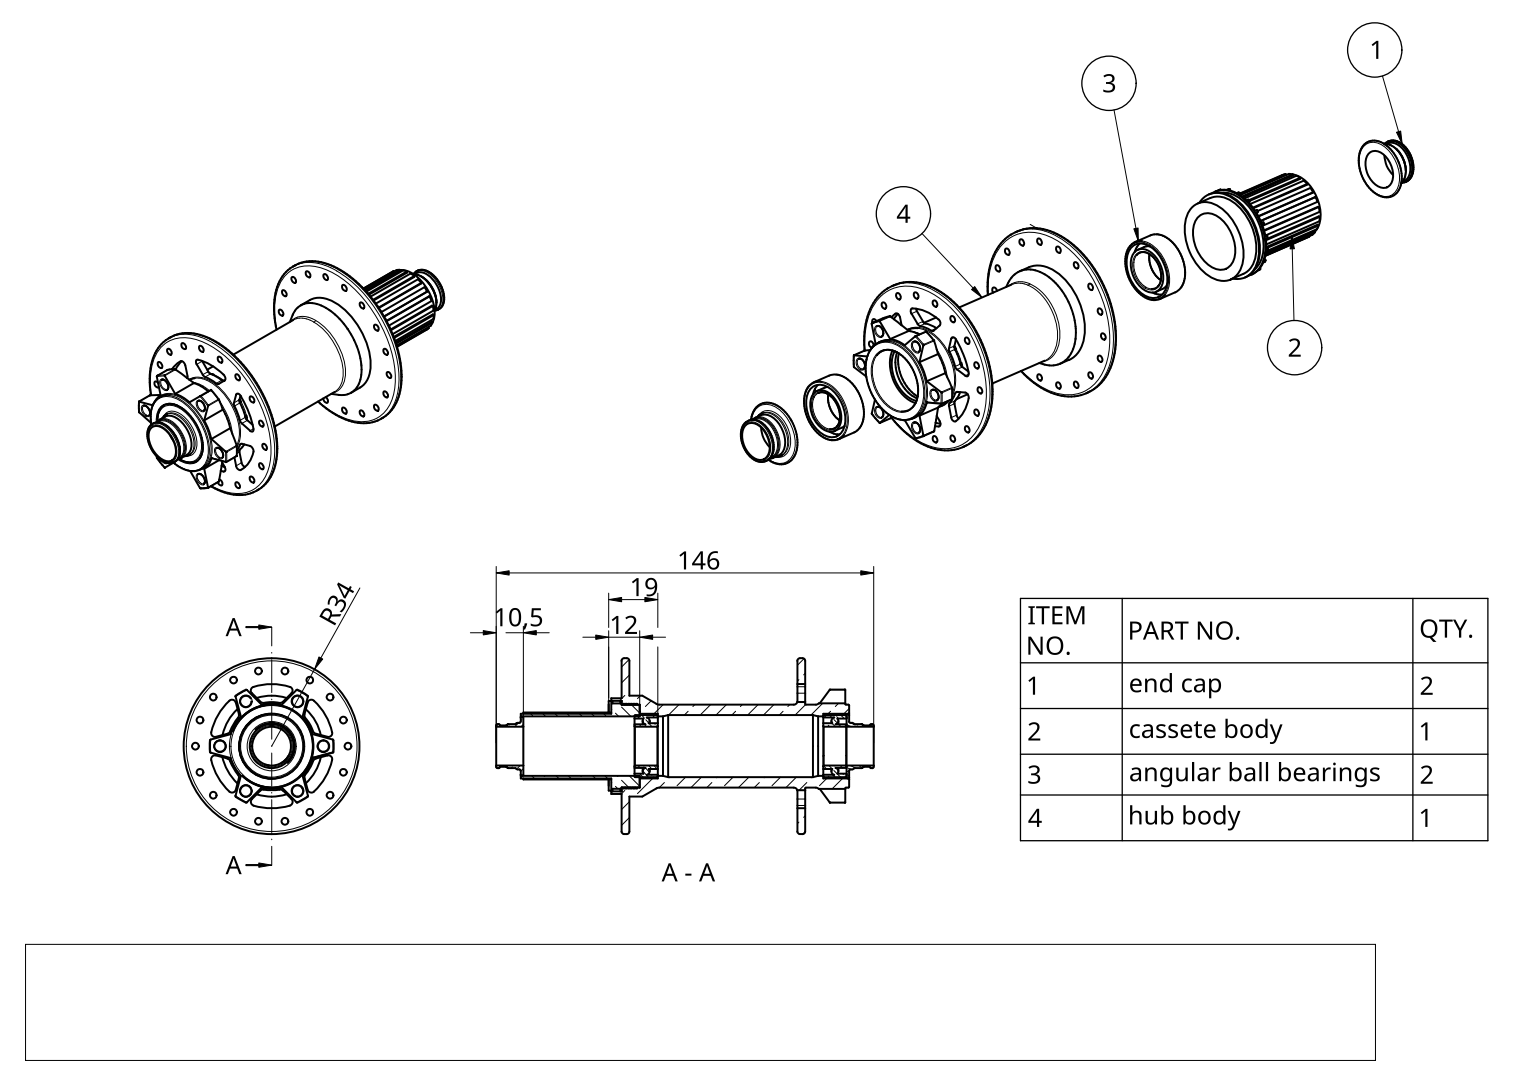
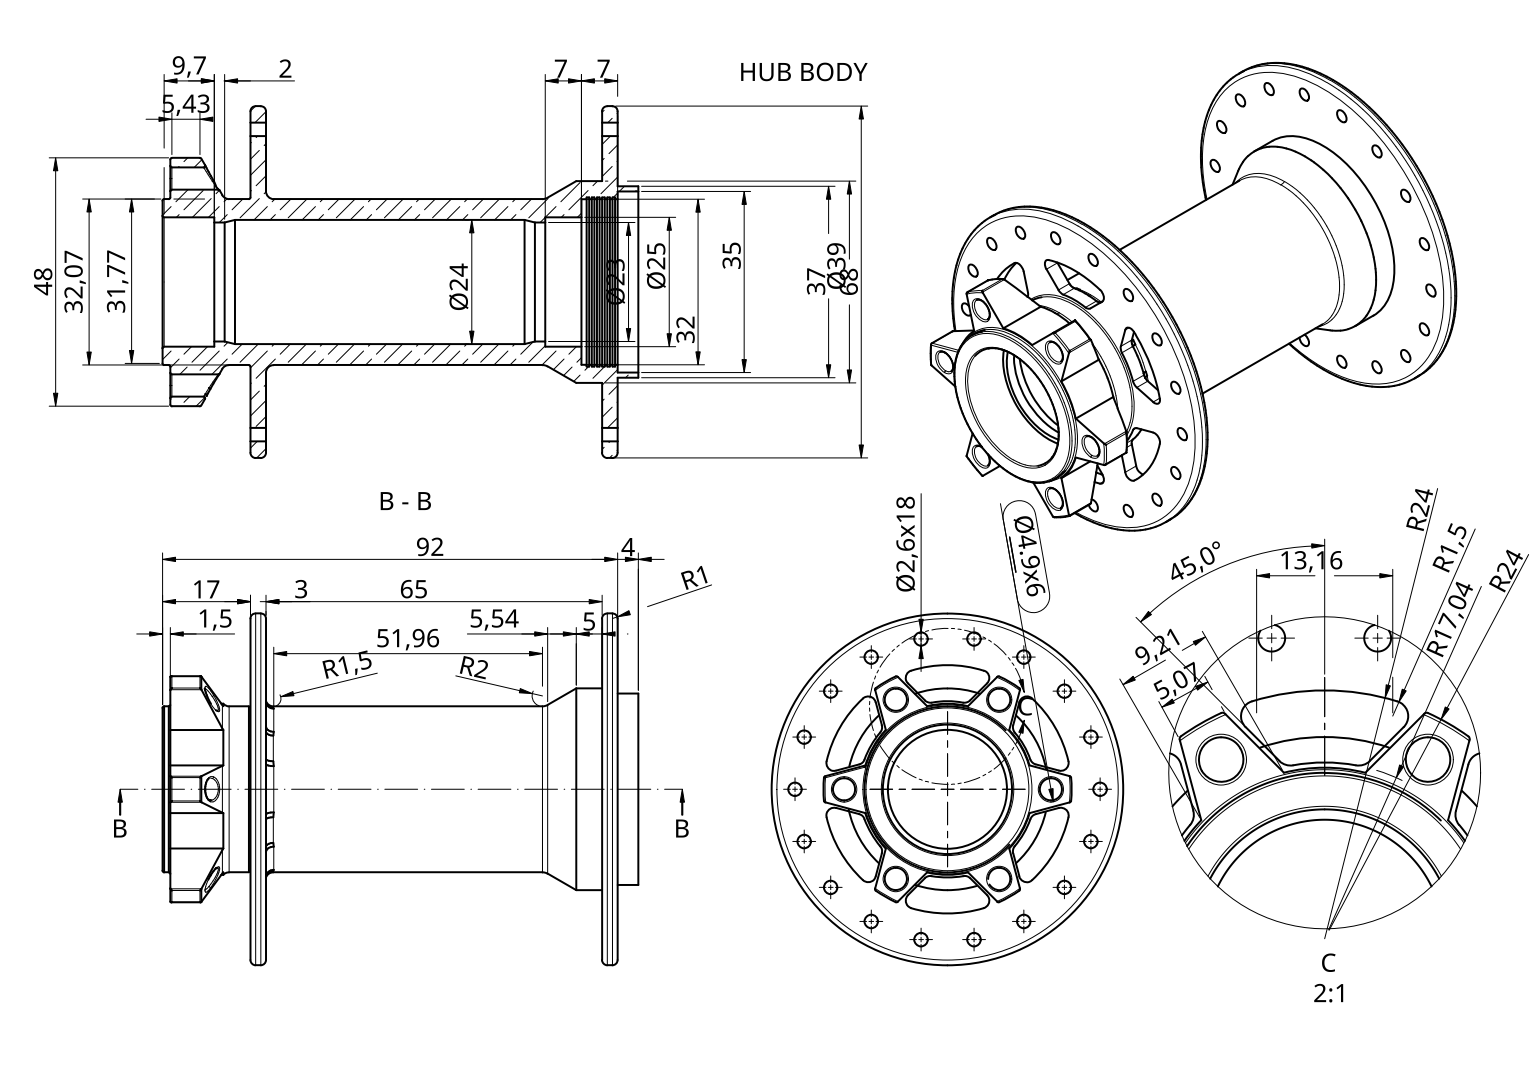
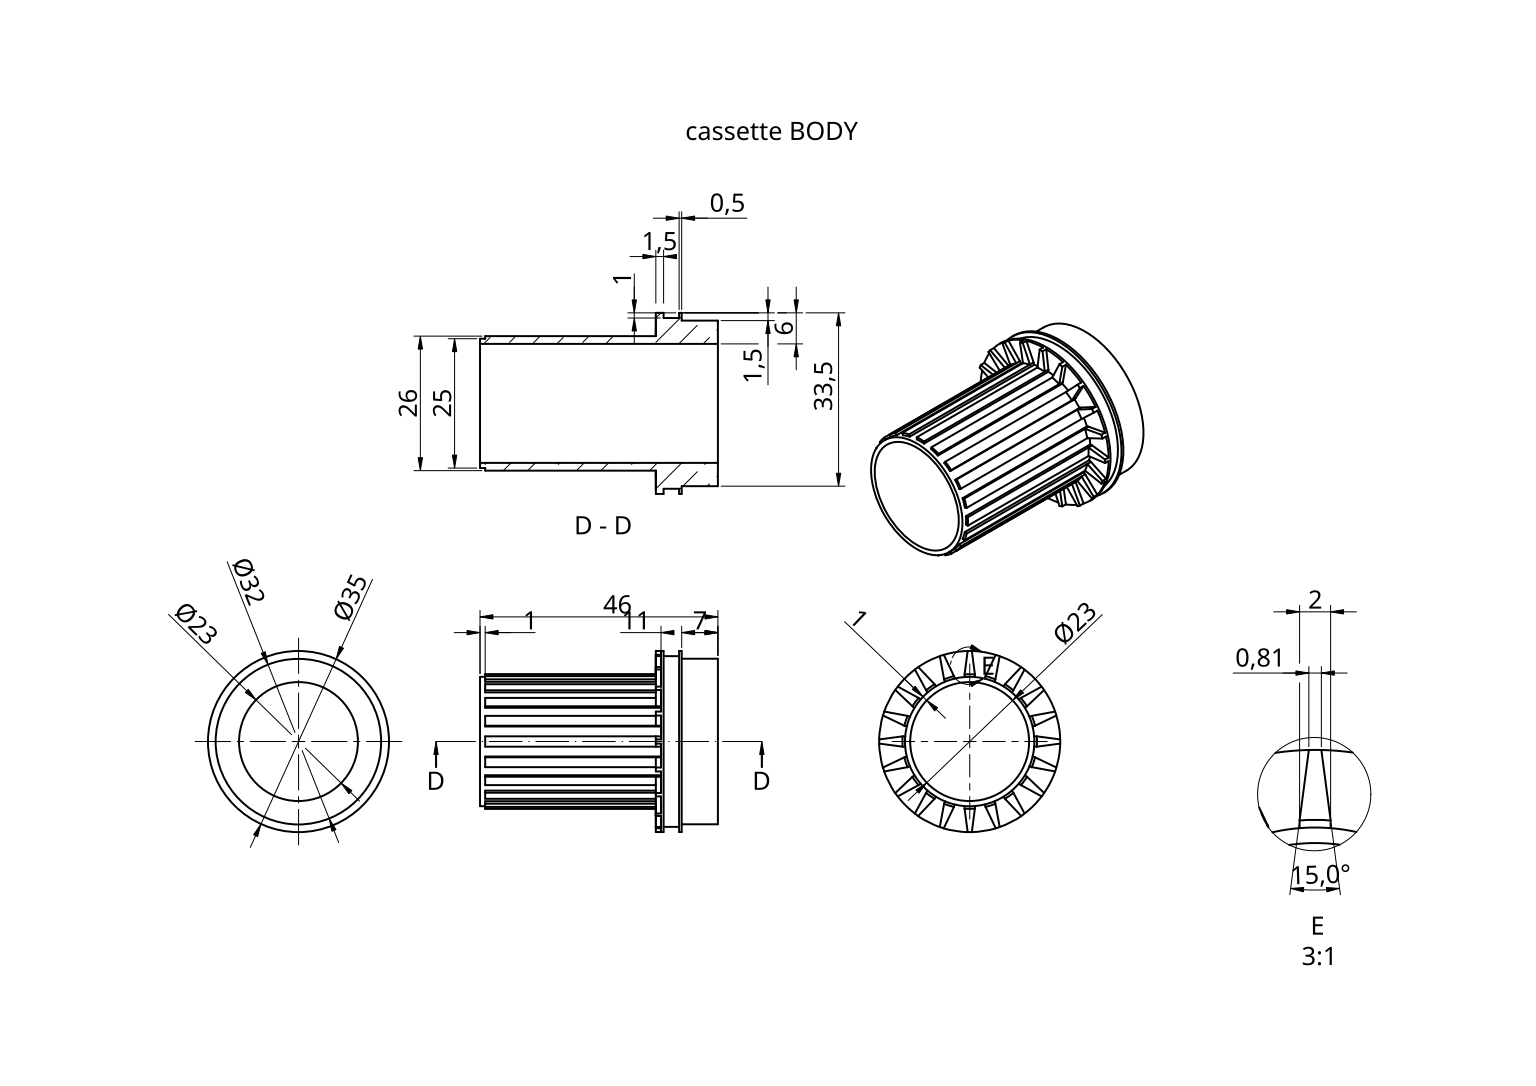
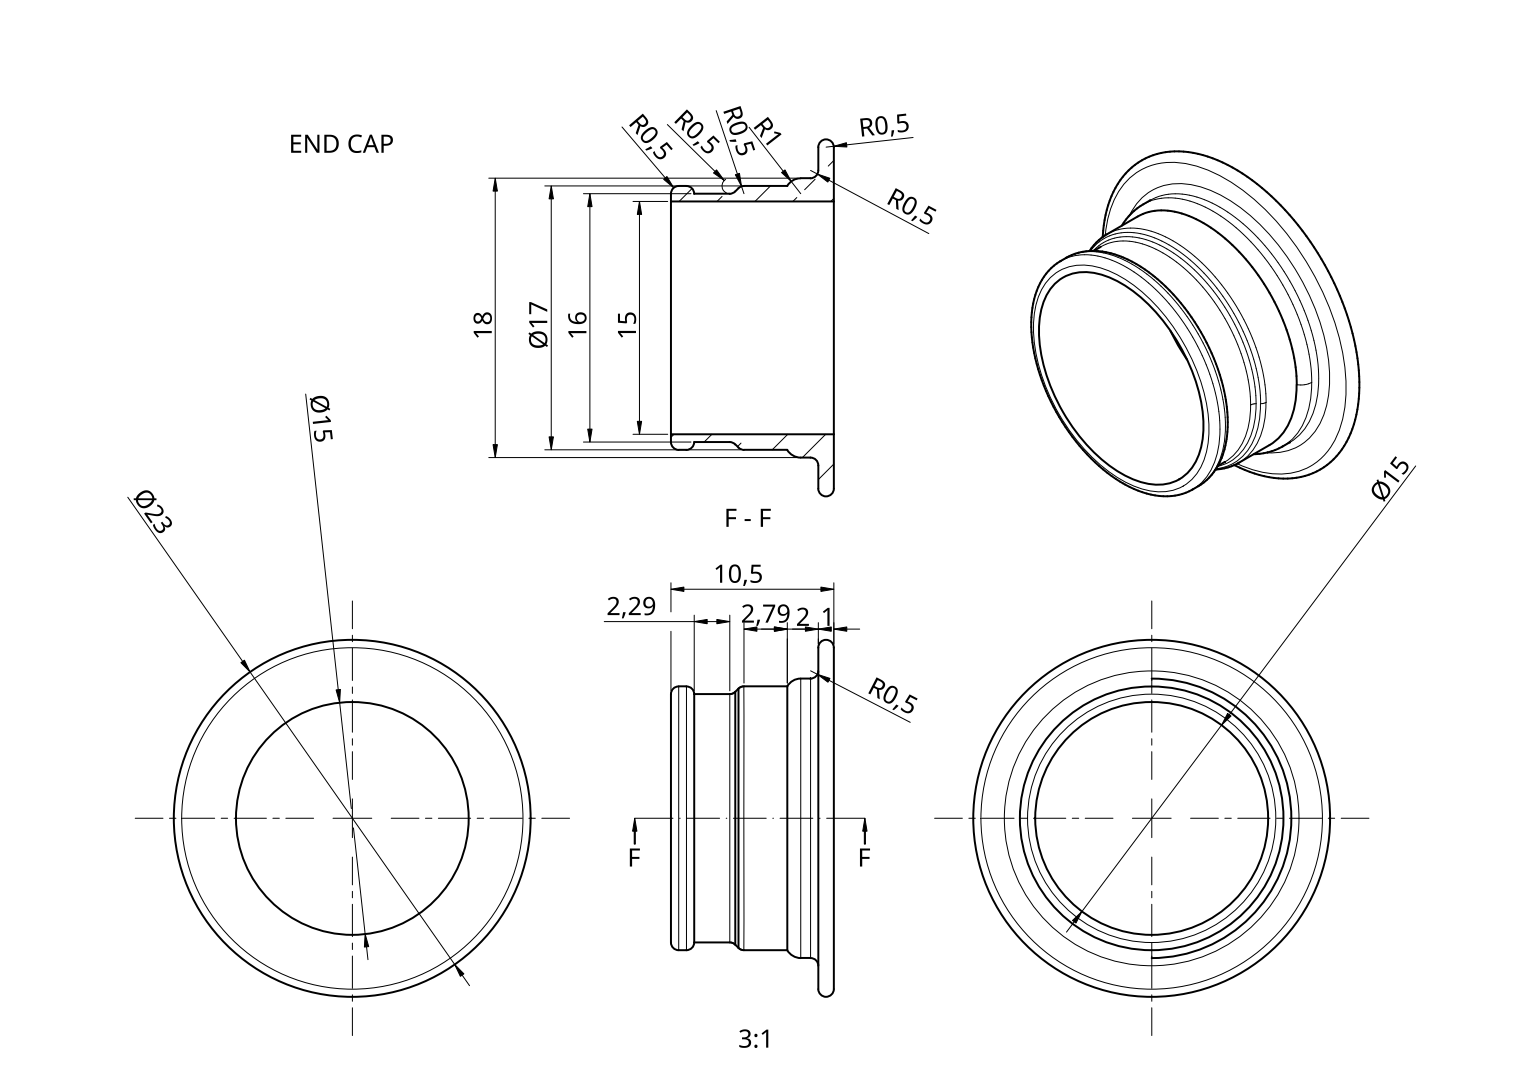
ISO-10303-21;
HEADER;
/* Generated by software containing ST-Developer
 * from STEP Tools, Inc. (www.steptools.com) 
 */
/* OPTION: using custom renumber hook */

FILE_DESCRIPTION(
/* description */ ('STEP AP242 Edition 2', 'CAx-IF Rec.Pracs.---Representation and Presentation of Product Manufa
cturing Information (PMI)---4.0---2014-10-13', 'CAx-IF Rec.Pracs.---3D Tessellated Geometry---0.4---2014-09-14', '2;1', 'CAx-IF Rec.Pracs.---User Defined Attributes---1.5---2016-08-15'),
/* implementation_level */ '2;1');

FILE_NAME(
/* name */ 'MAS-697',
/* time_stamp */ '2026-10-09T00:23:50Z',
/* author */ (''),
/* organization */ (''),
/* preprocessor_version */ 'ST-DEVELOPER v20',
/* originating_system */ 'ONSHAPE BY PTC INC, 1.221',
/* authorisation */ '  ');

FILE_SCHEMA (('AP242_MANAGED_MODEL_BASED_3D_ENGINEERING_MIM_LF { 1 0 10303 442 3 1 4 }'));
ENDSEC;

DATA;
#10=(
BOUNDED_SURFACE()
B_SPLINE_SURFACE(3,2,((#16553,#16554,#16555),(#16556,#16557,#16558),(#16559,
#16560,#16561),(#16562,#16563,#16564),(#16565,#16566,#16567),(#16568,#16569,
#16570),(#16571,#16572,#16573),(#16574,#16575,#16576),(#16577,#16578,#16579),
(#16580,#16581,#16582),(#16583,#16584,#16585),(#16586,#16587,#16588),(#16589,
#16590,#16591),(#16592,#16593,#16594),(#16595,#16596,#16597),(#16598,#16599,
#16600),(#16601,#16602,#16603),(#16604,#16605,#16606),(#16607,#16608,#16609),
(#16610,#16611,#16612),(#16613,#16614,#16615),(#16616,#16617,#16618),(#16619,
#16620,#16621),(#16622,#16623,#16624),(#16625,#16626,#16627),(#16628,#16629,
#16630),(#16631,#16632,#16633),(#16634,#16635,#16636),(#16637,#16638,#16639),
(#16640,#16641,#16642),(#16643,#16644,#16645),(#16646,#16647,#16648),(#16649,
#16650,#16651),(#16652,#16653,#16654),(#16655,#16656,#16657),(#16658,#16659,
#16660),(#16661,#16662,#16663),(#16664,#16665,#16666),(#16667,#16668,#16669),
(#16670,#16671,#16672),(#16673,#16674,#16675),(#16676,#16677,#16678),(#16679,
#16680,#16681),(#16682,#16683,#16684),(#16685,#16686,#16687),(#16688,#16689,
#16690),(#16691,#16692,#16693),(#16694,#16695,#16696),(#16697,#16698,#16699),
(#16700,#16701,#16702),(#16703,#16704,#16705),(#16706,#16707,#16708),(#16709,
#16710,#16711),(#16712,#16713,#16714),(#16715,#16716,#16717),(#16718,#16719,
#16720),(#16721,#16722,#16723),(#16724,#16725,#16726),(#16727,#16728,#16729),
(#16730,#16731,#16732),(#16733,#16734,#16735),(#16736,#16737,#16738),(#16739,
#16740,#16741),(#16742,#16743,#16744),(#16745,#16746,#16747),(#16748,#16749,
#16750)),.UNSPECIFIED.,.F.,.F.,.F.)
B_SPLINE_SURFACE_WITH_KNOTS((4,2,2,2,2,2,2,2,2,2,2,2,2,2,2,2,2,2,2,2,2,
2,2,2,2,2,2,2,2,2,2,2,4),(3,3),(0.,0.000514244430931465,0.00102848886186293,
0.0011570499695958,0.00128561107732866,0.00154273329279439,0.00205697772372586,
0.00218553883145873,0.00231409993919159,0.00257122215465732,0.00282834437012306,
0.00295690547785592,0.00308546658558879,0.00359971101652025,0.00372827212425312,
0.00385683323198599,0.00411395544745172,0.00424251655518458,0.00437107766291745,
0.00462819987838318,0.00488532209384892,0.00514244430931465,0.00565668874024611,
0.00591381095571184,0.00617093317117758,0.00668517760210904,0.00681373870984191,
0.00694229981757478,0.00719942203304051,0.00771366646397197,0.00784222757170484,
0.00797078867943771,0.00822791089490344),(0.,1.),.UNSPECIFIED.)
GEOMETRIC_REPRESENTATION_ITEM()
RATIONAL_B_SPLINE_SURFACE(((1.,0.727605019291272,1.),(1.,0.738269745261549,
1.),(1.,0.748592075286312,1.),(1.,0.768595657332798,1.),(1.,0.77827867017842,
1.),(1.,0.78996120454497,1.),(1.,0.792280826878612,1.),(1.,0.796828421990593,
1.),(1.,0.799061536127563,1.),(1.,0.805638929370508,1.),(1.,0.809861611074041,
1.),(1.,0.822031308701411,1.),(1.,0.829487589673691,1.),(1.,0.83785145435952,
1.),(1.,0.839480856802847,1.),(1.,0.842608559784881,1.),(1.,0.844105726044166,
1.),(1.,0.8483952491525,1.),(1.,0.850986216864091,1.),(1.,0.855606962686796,
1.),(1.,0.857636888703679,1.),(1.,0.860227819923722,1.),(1.,0.861017295679437,
1.),(1.,0.862419224745769,1.),(1.,0.863034322359247,1.),(1.,0.865683471685309,
1.),(1.,0.866451432203696,1.),(1.,0.865641730003757,1.),(1.,0.865389467353766,
1.),(1.,0.864714302219203,1.),(1.,0.864291039129295,1.),(1.,0.862771536048431,
1.),(1.,0.861426213021586,1.),(1.,0.858926691433347,1.),(1.,0.858013099107922,
1.),(1.,0.856026014492249,1.),(1.,0.854948935558792,1.),(1.,0.851506192237994,
1.),(1.,0.848937517425832,1.),(1.,0.843296974763866,1.),(1.,0.840224952153795,
1.),(1.,0.833601620182266,1.),(1.,0.830031077299106,1.),(1.,0.818809152212353,
1.),(1.,0.810636621270602,1.),(1.,0.797446978165117,1.),(1.,0.792872941755034,
1.),(1.,0.78353694939152,1.),(1.,0.778775433925334,1.),(1.,0.764221056564085,
1.),(1.,0.754161223208667,1.),(1.,0.741128124491465,1.),(1.,0.738495960101253,
1.),(1.,0.733227832409848,1.),(1.,0.730586739908481,1.),(1.,0.722641688562764,
1.),(1.,0.717316009840664,1.),(1.,0.701244534517323,1.),(1.,0.690405239081963,
1.),(1.,0.676661477613385,1.),(1.,0.673899376379498,1.),(1.,0.66840092468647,
1.),(1.,0.665659348664159,1.),(1.,0.657456353546285,1.),(1.,0.652016628878168,
1.),(1.,0.646603422936517,1.)))
REPRESENTATION_ITEM('')
SURFACE()
);
#11=(
BOUNDED_SURFACE()
B_SPLINE_SURFACE(3,2,((#16753,#16754,#16755),(#16756,#16757,#16758),(#16759,
#16760,#16761),(#16762,#16763,#16764),(#16765,#16766,#16767),(#16768,#16769,
#16770),(#16771,#16772,#16773),(#16774,#16775,#16776),(#16777,#16778,#16779),
(#16780,#16781,#16782),(#16783,#16784,#16785),(#16786,#16787,#16788),(#16789,
#16790,#16791),(#16792,#16793,#16794),(#16795,#16796,#16797),(#16798,#16799,
#16800),(#16801,#16802,#16803),(#16804,#16805,#16806),(#16807,#16808,#16809),
(#16810,#16811,#16812),(#16813,#16814,#16815),(#16816,#16817,#16818),(#16819,
#16820,#16821),(#16822,#16823,#16824),(#16825,#16826,#16827),(#16828,#16829,
#16830),(#16831,#16832,#16833),(#16834,#16835,#16836),(#16837,#16838,#16839),
(#16840,#16841,#16842),(#16843,#16844,#16845),(#16846,#16847,#16848),(#16849,
#16850,#16851),(#16852,#16853,#16854),(#16855,#16856,#16857),(#16858,#16859,
#16860),(#16861,#16862,#16863),(#16864,#16865,#16866),(#16867,#16868,#16869),
(#16870,#16871,#16872),(#16873,#16874,#16875),(#16876,#16877,#16878),(#16879,
#16880,#16881),(#16882,#16883,#16884),(#16885,#16886,#16887),(#16888,#16889,
#16890),(#16891,#16892,#16893),(#16894,#16895,#16896),(#16897,#16898,#16899),
(#16900,#16901,#16902),(#16903,#16904,#16905),(#16906,#16907,#16908),(#16909,
#16910,#16911),(#16912,#16913,#16914),(#16915,#16916,#16917),(#16918,#16919,
#16920),(#16921,#16922,#16923),(#16924,#16925,#16926)),.UNSPECIFIED.,.F.,
 .F.,.F.)
B_SPLINE_SURFACE_WITH_KNOTS((4,2,2,2,2,2,2,2,2,2,2,2,2,2,2,2,2,2,2,2,2,
2,2,2,2,2,2,2,4),(3,3),(0.00822791099999177,0.0087421553258349,0.00899927754130063,
0.00925639975676636,0.00951352197223209,0.00964208307996496,0.00977064418769782,
0.0102848886186293,0.010542010834095,0.0106705719418279,0.0107991330495608,
0.0113133774804922,0.011570499695958,0.0118276219114237,0.0120847441268894,
0.0123418663423552,0.0128561107732866,0.0129846718810195,0.0131132329887523,
0.0133703552042181,0.0136274774196838,0.0137560385274167,0.0138845996351495,
0.014398844066081,0.0146559662815467,0.0149130884970125,0.0154273329279439,
0.0159415773588754,0.0164558217898069),(0.,1.),.UNSPECIFIED.)
GEOMETRIC_REPRESENTATION_ITEM()
RATIONAL_B_SPLINE_SURFACE(((1.,0.646603416299741,1.),(1.,0.635777845415767,
1.),(1.,0.625055607928809,1.),(1.,0.609127621650672,1.),(1.,0.603886597603737,
1.),(1.,0.593641123894353,1.),(1.,0.588621119622323,1.),(1.,0.578794287069315,
1.),(1.,0.573987397424529,1.),(1.,0.566949594156529,1.),(1.,0.564632492256596,
1.),(1.,0.560059142358784,1.),(1.,0.557801592065244,1.),(1.,0.546803856262994,
1.),(1.,0.538816844550094,1.),(1.,0.528181154475445,1.),(1.,0.524861837914593,
1.),(1.,0.520257295698364,1.),(1.,0.518780914891828,1.),(1.,0.51599600081368,
1.),(1.,0.514683858232128,1.),(1.,0.508526013773749,1.),(1.,0.50487673783709,
1.),(1.,0.50148708526461,1.),(1.,0.500708624573298,1.),(1.,0.499919057301541,
1.),(1.,0.499897805772348,1.),(1.,0.500588074464456,1.),(1.,0.501299602522433,
1.),(1.,0.503460750293262,1.),(1.,0.504920849886873,1.),(1.,0.510276775109774,
1.),(1.,0.515155530687803,1.),(1.,0.522754639298001,1.),(1.,0.524354452613133,
1.),(1.,0.527668122842079,1.),(1.,0.529384771533693,1.),(1.,0.534705395354146,
1.),(1.,0.538479529845963,1.),(1.,0.546449215356828,1.),(1.,0.550644846474471,
1.),(1.,0.55724182544749,1.),(1.,0.559494088256891,1.),(1.,0.564052482183535,
1.),(1.,0.566363881497447,1.),(1.,0.578074130679415,1.),(1.,0.587926629008193,
1.),(1.,0.603363711869573,1.),(1.,0.608631647709976,1.),(1.,0.619200799287789,
1.),(1.,0.624523791984934,1.),(1.,0.640605786326143,1.),(1.,0.65147620310061,
1.),(1.,0.67354644028781,1.),(1.,0.684474150861673,1.),(1.,0.706154675135368,
1.),(1.,0.716910539945706,1.),(1.,0.727605019291272,1.)))
REPRESENTATION_ITEM('')
SURFACE()
);
#12=(
BOUNDED_SURFACE()
B_SPLINE_SURFACE(3,2,((#16928,#16929,#16930),(#16931,#16932,#16933),(#16934,
#16935,#16936),(#16937,#16938,#16939),(#16940,#16941,#16942),(#16943,#16944,
#16945),(#16946,#16947,#16948),(#16949,#16950,#16951),(#16952,#16953,#16954),
(#16955,#16956,#16957),(#16958,#16959,#16960),(#16961,#16962,#16963),(#16964,
#16965,#16966),(#16967,#16968,#16969),(#16970,#16971,#16972),(#16973,#16974,
#16975),(#16976,#16977,#16978),(#16979,#16980,#16981),(#16982,#16983,#16984),
(#16985,#16986,#16987),(#16988,#16989,#16990),(#16991,#16992,#16993),(#16994,
#16995,#16996),(#16997,#16998,#16999),(#17000,#17001,#17002),(#17003,#17004,
#17005),(#17006,#17007,#17008),(#17009,#17010,#17011),(#17012,#17013,#17014),
(#17015,#17016,#17017),(#17018,#17019,#17020),(#17021,#17022,#17023),(#17024,
#17025,#17026),(#17027,#17028,#17029),(#17030,#17031,#17032),(#17033,#17034,
#17035),(#17036,#17037,#17038),(#17039,#17040,#17041),(#17042,#17043,#17044),
(#17045,#17046,#17047),(#17048,#17049,#17050),(#17051,#17052,#17053),(#17054,
#17055,#17056),(#17057,#17058,#17059),(#17060,#17061,#17062),(#17063,#17064,
#17065),(#17066,#17067,#17068),(#17069,#17070,#17071),(#17072,#17073,#17074),
(#17075,#17076,#17077),(#17078,#17079,#17080),(#17081,#17082,#17083),(#17084,
#17085,#17086),(#17087,#17088,#17089),(#17090,#17091,#17092),(#17093,#17094,
#17095),(#17096,#17097,#17098),(#17099,#17100,#17101),(#17102,#17103,#17104),
(#17105,#17106,#17107),(#17108,#17109,#17110),(#17111,#17112,#17113),(#17114,
#17115,#17116),(#17117,#17118,#17119),(#17120,#17121,#17122),(#17123,#17124,
#17125)),.UNSPECIFIED.,.F.,.F.,.F.)
B_SPLINE_SURFACE_WITH_KNOTS((4,2,2,2,2,2,2,2,2,2,2,2,2,2,2,2,2,2,2,2,2,
2,2,2,2,2,2,2,2,2,2,2,4),(3,3),(0.,0.000514244430931465,0.00102848886186293,
0.0011570499695958,0.00128561107732866,0.00154273329279439,0.00205697772372586,
0.00218553883145873,0.00231409993919159,0.00257122215465732,0.00282834437012306,
0.00295690547785592,0.00308546658558879,0.00359971101652025,0.00372827212425312,
0.00385683323198599,0.00411395544745172,0.00424251655518459,0.00437107766291745,
0.00462819987838319,0.00488532209384892,0.00514244430931465,0.00565668874024611,
0.00591381095571185,0.00617093317117758,0.00668517760210904,0.00681373870984191,
0.00694229981757478,0.00719942203304051,0.00771366646397197,0.00784222757170484,
0.00797078867943771,0.00822791089490344),(0.,1.),.UNSPECIFIED.)
GEOMETRIC_REPRESENTATION_ITEM()
RATIONAL_B_SPLINE_SURFACE(((1.,0.727605019291273,1.),(1.,0.738269745261463,
1.),(1.,0.748592075286425,1.),(1.,0.768595657332682,1.),(1.,0.778278670178458,
1.),(1.,0.78996120454496,1.),(1.,0.792280826878572,1.),(1.,0.79682842199063,
1.),(1.,0.799061536127604,1.),(1.,0.805638929370428,1.),(1.,0.809861611074089,
1.),(1.,0.822031308701317,1.),(1.,0.829487589673701,1.),(1.,0.837851454359518,
1.),(1.,0.839480856802835,1.),(1.,0.842608559784893,1.),(1.,0.84410572604416,
1.),(1.,0.848395249152509,1.),(1.,0.850986216864149,1.),(1.,0.85560696268674,
1.),(1.,0.857636888703671,1.),(1.,0.860227819923728,1.),(1.,0.861017295679411,
1.),(1.,0.862419224745796,1.),(1.,0.863034322359203,1.),(1.,0.865683471685481,
1.),(1.,0.86645143220361,1.),(1.,0.865641730003779,1.),(1.,0.865389467353773,
1.),(1.,0.864714302219195,1.),(1.,0.864291039129257,1.),(1.,0.862771536048502,
1.),(1.,0.861426213021595,1.),(1.,0.858926691433342,1.),(1.,0.858013099107929,
1.),(1.,0.856026014492242,1.),(1.,0.854948935558757,1.),(1.,0.851506192238061,
1.),(1.,0.848937517425937,1.),(1.,0.84329697476376,1.),(1.,0.84022495215382,
1.),(1.,0.833601620182241,1.),(1.,0.830031077299101,1.),(1.,0.818809152212363,
1.),(1.,0.810636621270581,1.),(1.,0.797446978165125,1.),(1.,0.792872941755087,
1.),(1.,0.783536949391466,1.),(1.,0.778775433925213,1.),(1.,0.764221056564323,
1.),(1.,0.754161223208549,1.),(1.,0.741128124491493,1.),(1.,0.738495960101291,
1.),(1.,0.73322783240981,1.),(1.,0.73058673990848,1.),(1.,0.722641688562763,
1.),(1.,0.717316009840587,1.),(1.,0.701244534517476,1.),(1.,0.690405239082108,
1.),(1.,0.676661477613348,1.),(1.,0.673899376379507,1.),(1.,0.66840092468646,
1.),(1.,0.665659348664103,1.),(1.,0.657456353546395,1.),(1.,0.652016628878089,
1.),(1.,0.646603422936514,1.)))
REPRESENTATION_ITEM('')
SURFACE()
);
#13=(
BOUNDED_SURFACE()
B_SPLINE_SURFACE(3,2,((#17128,#17129,#17130),(#17131,#17132,#17133),(#17134,
#17135,#17136),(#17137,#17138,#17139),(#17140,#17141,#17142),(#17143,#17144,
#17145),(#17146,#17147,#17148),(#17149,#17150,#17151),(#17152,#17153,#17154),
(#17155,#17156,#17157),(#17158,#17159,#17160),(#17161,#17162,#17163),(#17164,
#17165,#17166),(#17167,#17168,#17169),(#17170,#17171,#17172),(#17173,#17174,
#17175),(#17176,#17177,#17178),(#17179,#17180,#17181),(#17182,#17183,#17184),
(#17185,#17186,#17187),(#17188,#17189,#17190),(#17191,#17192,#17193),(#17194,
#17195,#17196),(#17197,#17198,#17199),(#17200,#17201,#17202),(#17203,#17204,
#17205),(#17206,#17207,#17208),(#17209,#17210,#17211),(#17212,#17213,#17214),
(#17215,#17216,#17217),(#17218,#17219,#17220),(#17221,#17222,#17223),(#17224,
#17225,#17226),(#17227,#17228,#17229),(#17230,#17231,#17232),(#17233,#17234,
#17235),(#17236,#17237,#17238),(#17239,#17240,#17241),(#17242,#17243,#17244),
(#17245,#17246,#17247),(#17248,#17249,#17250),(#17251,#17252,#17253),(#17254,
#17255,#17256),(#17257,#17258,#17259),(#17260,#17261,#17262),(#17263,#17264,
#17265),(#17266,#17267,#17268),(#17269,#17270,#17271),(#17272,#17273,#17274),
(#17275,#17276,#17277),(#17278,#17279,#17280),(#17281,#17282,#17283),(#17284,
#17285,#17286),(#17287,#17288,#17289),(#17290,#17291,#17292),(#17293,#17294,
#17295),(#17296,#17297,#17298),(#17299,#17300,#17301)),.UNSPECIFIED.,.F.,
 .F.,.F.)
B_SPLINE_SURFACE_WITH_KNOTS((4,2,2,2,2,2,2,2,2,2,2,2,2,2,2,2,2,2,2,2,2,
2,2,2,2,2,2,2,4),(3,3),(0.00822791099999177,0.0087421553258349,0.00899927754130063,
0.00925639975676636,0.0095135219722321,0.00964208307996496,0.00977064418769783,
0.0102848886186293,0.010542010834095,0.0106705719418279,0.0107991330495608,
0.0113133774804922,0.011570499695958,0.0118276219114237,0.0120847441268894,
0.0123418663423552,0.0128561107732866,0.0129846718810195,0.0131132329887524,
0.0133703552042181,0.0136274774196838,0.0137560385274167,0.0138845996351495,
0.014398844066081,0.0146559662815467,0.0149130884970125,0.0154273329279439,
0.0159415773588754,0.0164558217898069),(0.,1.),.UNSPECIFIED.)
GEOMETRIC_REPRESENTATION_ITEM()
RATIONAL_B_SPLINE_SURFACE(((1.,0.646603416299739,1.),(1.,0.635777845415872,
1.),(1.,0.625055607928666,1.),(1.,0.609127621650746,1.),(1.,0.603886597603766,
1.),(1.,0.593641123894325,1.),(1.,0.588621119622213,1.),(1.,0.578794287069424,
1.),(1.,0.573987397424613,1.),(1.,0.566949594156483,1.),(1.,0.564632492256567,
1.),(1.,0.560059142358813,1.),(1.,0.557801592065364,1.),(1.,0.546803856262498,
1.),(1.,0.538816844550381,1.),(1.,0.528181154475289,1.),(1.,0.524861837914536,
1.),(1.,0.520257295698394,1.),(1.,0.518780914891774,1.),(1.,0.515996000813732,
1.),(1.,0.514683858232152,1.),(1.,0.508526013773653,1.),(1.,0.504876737837329,
1.),(1.,0.501487085264488,1.),(1.,0.500708624573413,1.),(1.,0.499919057301424,
1.),(1.,0.499897805772289,1.),(1.,0.500588074464511,1.),(1.,0.501299602522455,
1.),(1.,0.503460750293236,1.),(1.,0.504920849887092,1.),(1.,0.510276775109342,
1.),(1.,0.515155530687803,1.),(1.,0.522754639298001,1.),(1.,0.52435445261312,
1.),(1.,0.527668122842095,1.),(1.,0.529384771533763,1.),(1.,0.534705395354007,
1.),(1.,0.538479529845905,1.),(1.,0.546449215356886,1.),(1.,0.550644846474304,
1.),(1.,0.55724182544757,1.),(1.,0.559494088256935,1.),(1.,0.564052482183492,
1.),(1.,0.566363881497433,1.),(1.,0.578074130679462,1.),(1.,0.587926629008058,
1.),(1.,0.603363711869641,1.),(1.,0.608631647710066,1.),(1.,0.619200799287697,
1.),(1.,0.624523791984965,1.),(1.,0.640605786326088,1.),(1.,0.651476203100892,
1.),(1.,0.67354644028753,1.),(1.,0.684474150861655,1.),(1.,0.706154675135388,
1.),(1.,0.716910539945691,1.),(1.,0.727605019291273,1.)))
REPRESENTATION_ITEM('')
SURFACE()
);
#14=(
BOUNDED_SURFACE()
B_SPLINE_SURFACE(3,2,((#17308,#17309,#17310),(#17311,#17312,#17313),(#17314,
#17315,#17316),(#17317,#17318,#17319),(#17320,#17321,#17322),(#17323,#17324,
#17325),(#17326,#17327,#17328),(#17329,#17330,#17331),(#17332,#17333,#17334),
(#17335,#17336,#17337),(#17338,#17339,#17340),(#17341,#17342,#17343),(#17344,
#17345,#17346),(#17347,#17348,#17349),(#17350,#17351,#17352),(#17353,#17354,
#17355),(#17356,#17357,#17358),(#17359,#17360,#17361),(#17362,#17363,#17364),
(#17365,#17366,#17367),(#17368,#17369,#17370),(#17371,#17372,#17373),(#17374,
#17375,#17376),(#17377,#17378,#17379),(#17380,#17381,#17382),(#17383,#17384,
#17385),(#17386,#17387,#17388),(#17389,#17390,#17391),(#17392,#17393,#17394),
(#17395,#17396,#17397),(#17398,#17399,#17400),(#17401,#17402,#17403),(#17404,
#17405,#17406),(#17407,#17408,#17409),(#17410,#17411,#17412),(#17413,#17414,
#17415),(#17416,#17417,#17418),(#17419,#17420,#17421),(#17422,#17423,#17424),
(#17425,#17426,#17427),(#17428,#17429,#17430),(#17431,#17432,#17433),(#17434,
#17435,#17436),(#17437,#17438,#17439),(#17440,#17441,#17442),(#17443,#17444,
#17445),(#17446,#17447,#17448),(#17449,#17450,#17451),(#17452,#17453,#17454),
(#17455,#17456,#17457),(#17458,#17459,#17460),(#17461,#17462,#17463),(#17464,
#17465,#17466),(#17467,#17468,#17469),(#17470,#17471,#17472),(#17473,#17474,
#17475),(#17476,#17477,#17478),(#17479,#17480,#17481),(#17482,#17483,#17484),
(#17485,#17486,#17487),(#17488,#17489,#17490),(#17491,#17492,#17493),(#17494,
#17495,#17496),(#17497,#17498,#17499),(#17500,#17501,#17502),(#17503,#17504,
#17505)),.UNSPECIFIED.,.F.,.F.,.F.)
B_SPLINE_SURFACE_WITH_KNOTS((4,2,2,2,2,2,2,2,2,2,2,2,2,2,2,2,2,2,2,2,2,
2,2,2,2,2,2,2,2,2,2,2,4),(3,3),(0.,0.000514244430931465,0.00102848886186293,
0.0011570499695958,0.00128561107732866,0.00154273329279439,0.00205697772372586,
0.00218553883145873,0.00231409993919159,0.00257122215465732,0.00282834437012306,
0.00295690547785592,0.00308546658558879,0.00359971101652025,0.00372827212425312,
0.00385683323198599,0.00411395544745172,0.00424251655518459,0.00437107766291745,
0.00462819987838319,0.00488532209384892,0.00514244430931465,0.00565668874024611,
0.00591381095571185,0.00617093317117758,0.00668517760210904,0.00681373870984191,
0.00694229981757478,0.00719942203304051,0.00771366646397197,0.00784222757170484,
0.00797078867943771,0.00822791089490344),(0.,1.),.UNSPECIFIED.)
GEOMETRIC_REPRESENTATION_ITEM()
RATIONAL_B_SPLINE_SURFACE(((1.,0.727605019291271,1.),(1.,0.738269745261525,
1.),(1.,0.748592075286343,1.),(1.,0.768595657332771,1.),(1.,0.778278670178227,
1.),(1.,0.789961204545018,1.),(1.,0.792280826878548,1.),(1.,0.796828421990654,
1.),(1.,0.799061536127593,1.),(1.,0.805638929370445,1.),(1.,0.809861611074169,
1.),(1.,0.822031308701155,1.),(1.,0.82948758967367,1.),(1.,0.837851454359524,
1.),(1.,0.839480856802831,1.),(1.,0.842608559784899,1.),(1.,0.844105726044111,
1.),(1.,0.848395249152611,1.),(1.,0.850986216864154,1.),(1.,0.855606962686734,
1.),(1.,0.85763688870368,1.),(1.,0.860227819923723,1.),(1.,0.861017295679384,
1.),(1.,0.862419224745822,1.),(1.,0.863034322359218,1.),(1.,0.865683471685424,
1.),(1.,0.866451432203608,1.),(1.,0.865641730003778,1.),(1.,0.865389467353742,
1.),(1.,0.864714302219227,1.),(1.,0.86429103912928,1.),(1.,0.862771536048459,
1.),(1.,0.861426213021567,1.),(1.,0.858926691433357,1.),(1.,0.858013099107913,
1.),(1.,0.856026014492259,1.),(1.,0.854948935558786,1.),(1.,0.851506192238003,
1.),(1.,0.848937517425855,1.),(1.,0.843296974763842,1.),(1.,0.840224952153848,
1.),(1.,0.833601620182212,1.),(1.,0.830031077299101,1.),(1.,0.818809152212363,
1.),(1.,0.810636621270486,1.),(1.,0.797446978165174,1.),(1.,0.792872941755086,
1.),(1.,0.783536949391466,1.),(1.,0.778775433925242,1.),(1.,0.764221056564266,
1.),(1.,0.754161223208754,1.),(1.,0.741128124491444,1.),(1.,0.738495960101248,
1.),(1.,0.733227832409853,1.),(1.,0.730586739908468,1.),(1.,0.722641688562787,
1.),(1.,0.717316009840591,1.),(1.,0.701244534517466,1.),(1.,0.69040523908203,
1.),(1.,0.676661477613367,1.),(1.,0.67389937637949,1.),(1.,0.668400924686476,
1.),(1.,0.665659348664088,1.),(1.,0.65745635354643,1.),(1.,0.652016628878062,
1.),(1.,0.646603422936515,1.)))
REPRESENTATION_ITEM('')
SURFACE()
);
#15=(
BOUNDED_SURFACE()
B_SPLINE_SURFACE(3,2,((#17508,#17509,#17510),(#17511,#17512,#17513),(#17514,
#17515,#17516),(#17517,#17518,#17519),(#17520,#17521,#17522),(#17523,#17524,
#17525),(#17526,#17527,#17528),(#17529,#17530,#17531),(#17532,#17533,#17534),
(#17535,#17536,#17537),(#17538,#17539,#17540),(#17541,#17542,#17543),(#17544,
#17545,#17546),(#17547,#17548,#17549),(#17550,#17551,#17552),(#17553,#17554,
#17555),(#17556,#17557,#17558),(#17559,#17560,#17561),(#17562,#17563,#17564),
(#17565,#17566,#17567),(#17568,#17569,#17570),(#17571,#17572,#17573),(#17574,
#17575,#17576),(#17577,#17578,#17579),(#17580,#17581,#17582),(#17583,#17584,
#17585),(#17586,#17587,#17588),(#17589,#17590,#17591),(#17592,#17593,#17594),
(#17595,#17596,#17597),(#17598,#17599,#17600),(#17601,#17602,#17603),(#17604,
#17605,#17606),(#17607,#17608,#17609),(#17610,#17611,#17612),(#17613,#17614,
#17615),(#17616,#17617,#17618),(#17619,#17620,#17621),(#17622,#17623,#17624),
(#17625,#17626,#17627),(#17628,#17629,#17630),(#17631,#17632,#17633),(#17634,
#17635,#17636),(#17637,#17638,#17639),(#17640,#17641,#17642),(#17643,#17644,
#17645),(#17646,#17647,#17648),(#17649,#17650,#17651),(#17652,#17653,#17654),
(#17655,#17656,#17657),(#17658,#17659,#17660),(#17661,#17662,#17663),(#17664,
#17665,#17666),(#17667,#17668,#17669),(#17670,#17671,#17672),(#17673,#17674,
#17675),(#17676,#17677,#17678),(#17679,#17680,#17681)),.UNSPECIFIED.,.F.,
 .F.,.F.)
B_SPLINE_SURFACE_WITH_KNOTS((4,2,2,2,2,2,2,2,2,2,2,2,2,2,2,2,2,2,2,2,2,
2,2,2,2,2,2,2,4),(3,3),(0.00822791099999177,0.0087421553258349,0.00899927754130063,
0.00925639975676637,0.0095135219722321,0.00964208307996496,0.00977064418769783,
0.0102848886186293,0.010542010834095,0.0106705719418279,0.0107991330495608,
0.0113133774804922,0.011570499695958,0.0118276219114237,0.0120847441268894,
0.0123418663423552,0.0128561107732866,0.0129846718810195,0.0131132329887524,
0.0133703552042181,0.0136274774196838,0.0137560385274167,0.0138845996351496,
0.014398844066081,0.0146559662815468,0.0149130884970125,0.015427332927944,
0.0159415773588754,0.0164558217898069),(0.,1.),.UNSPECIFIED.)
GEOMETRIC_REPRESENTATION_ITEM()
RATIONAL_B_SPLINE_SURFACE(((1.,0.646603416299741,1.),(1.,0.635777845415857,
1.),(1.,0.625055607928685,1.),(1.,0.609127621650736,1.),(1.,0.603886597603802,
1.),(1.,0.593641123894284,1.),(1.,0.588621119622386,1.),(1.,0.578794287069253,
1.),(1.,0.573987397424614,1.),(1.,0.566949594156484,1.),(1.,0.564632492256556,
1.),(1.,0.560059142358826,1.),(1.,0.557801592065362,1.),(1.,0.546803856262521,
1.),(1.,0.538816844550013,1.),(1.,0.528181154475479,1.),(1.,0.524861837914558,
1.),(1.,0.52025729569838,1.),(1.,0.518780914891758,1.),(1.,0.51599600081375,
1.),(1.,0.514683858232071,1.),(1.,0.50852601377398,1.),(1.,0.504876737836812,
1.),(1.,0.50148708526475,1.),(1.,0.500708624573357,1.),(1.,0.499919057301484,
1.),(1.,0.499897805772248,1.),(1.,0.500588074464557,1.),(1.,0.501299602522294,
1.),(1.,0.503460750293403,1.),(1.,0.504920849886794,1.),(1.,0.510276775109926,
1.),(1.,0.515155530687822,1.),(1.,0.522754639297996,1.),(1.,0.524354452613109,
1.),(1.,0.527668122842108,1.),(1.,0.529384771533807,1.),(1.,0.534705395353914,
1.),(1.,0.538479529846021,1.),(1.,0.546449215356772,1.),(1.,0.550644846474468,
1.),(1.,0.557241825447494,1.),(1.,0.559494088256949,1.),(1.,0.564052482183478,
1.),(1.,0.566363881497384,1.),(1.,0.578074130679665,1.),(1.,0.587926629008355,
1.),(1.,0.603363711869489,1.),(1.,0.608631647709893,1.),(1.,0.61920079928787,
1.),(1.,0.624523791984875,1.),(1.,0.640605786326271,1.),(1.,0.651476203100745,
1.),(1.,0.673546440287674,1.),(1.,0.684474150861577,1.),(1.,0.706154675135463,
1.),(1.,0.716910539945636,1.),(1.,0.727605019291271,1.)))
REPRESENTATION_ITEM('')
SURFACE()
);
#16=(
BOUNDED_SURFACE()
B_SPLINE_SURFACE(3,2,((#17683,#17684,#17685),(#17686,#17687,#17688),(#17689,
#17690,#17691),(#17692,#17693,#17694),(#17695,#17696,#17697),(#17698,#17699,
#17700),(#17701,#17702,#17703),(#17704,#17705,#17706),(#17707,#17708,#17709),
(#17710,#17711,#17712),(#17713,#17714,#17715),(#17716,#17717,#17718),(#17719,
#17720,#17721),(#17722,#17723,#17724),(#17725,#17726,#17727),(#17728,#17729,
#17730),(#17731,#17732,#17733),(#17734,#17735,#17736),(#17737,#17738,#17739),
(#17740,#17741,#17742),(#17743,#17744,#17745),(#17746,#17747,#17748),(#17749,
#17750,#17751),(#17752,#17753,#17754),(#17755,#17756,#17757),(#17758,#17759,
#17760),(#17761,#17762,#17763),(#17764,#17765,#17766),(#17767,#17768,#17769),
(#17770,#17771,#17772),(#17773,#17774,#17775),(#17776,#17777,#17778),(#17779,
#17780,#17781),(#17782,#17783,#17784),(#17785,#17786,#17787),(#17788,#17789,
#17790),(#17791,#17792,#17793),(#17794,#17795,#17796),(#17797,#17798,#17799),
(#17800,#17801,#17802),(#17803,#17804,#17805),(#17806,#17807,#17808),(#17809,
#17810,#17811),(#17812,#17813,#17814),(#17815,#17816,#17817),(#17818,#17819,
#17820),(#17821,#17822,#17823),(#17824,#17825,#17826),(#17827,#17828,#17829),
(#17830,#17831,#17832),(#17833,#17834,#17835),(#17836,#17837,#17838),(#17839,
#17840,#17841),(#17842,#17843,#17844),(#17845,#17846,#17847),(#17848,#17849,
#17850),(#17851,#17852,#17853),(#17854,#17855,#17856),(#17857,#17858,#17859),
(#17860,#17861,#17862),(#17863,#17864,#17865),(#17866,#17867,#17868),(#17869,
#17870,#17871),(#17872,#17873,#17874),(#17875,#17876,#17877),(#17878,#17879,
#17880)),.UNSPECIFIED.,.F.,.F.,.F.)
B_SPLINE_SURFACE_WITH_KNOTS((4,2,2,2,2,2,2,2,2,2,2,2,2,2,2,2,2,2,2,2,2,
2,2,2,2,2,2,2,2,2,2,2,4),(3,3),(0.,0.000514244430931465,0.00102848886186293,
0.0011570499695958,0.00128561107732866,0.0015427332927944,0.00205697772372586,
0.00218553883145873,0.00231409993919159,0.00257122215465733,0.00282834437012306,
0.00295690547785592,0.00308546658558879,0.00359971101652026,0.00372827212425312,
0.00385683323198599,0.00411395544745172,0.00424251655518459,0.00437107766291745,
0.00462819987838319,0.00488532209384892,0.00514244430931465,0.00565668874024612,
0.00591381095571185,0.00617093317117758,0.00668517760210905,0.00681373870984191,
0.00694229981757478,0.00719942203304051,0.00771366646397198,0.00784222757170484,
0.00797078867943771,0.00822791089490344),(0.,1.),.UNSPECIFIED.)
GEOMETRIC_REPRESENTATION_ITEM()
RATIONAL_B_SPLINE_SURFACE(((1.,0.727605019291271,1.),(1.,0.73826974526155,
1.),(1.,0.748592075286311,1.),(1.,0.768595657332797,1.),(1.,0.778278670178333,
1.),(1.,0.789961204544991,1.),(1.,0.792280826878628,1.),(1.,0.796828421990575,
1.),(1.,0.799061536127595,1.),(1.,0.805638929370441,1.),(1.,0.809861611074004,
1.),(1.,0.822031308701488,1.),(1.,0.829487589673555,1.),(1.,0.837851454359553,
1.),(1.,0.839480856802828,1.),(1.,0.842608559784896,1.),(1.,0.844105726044104,
1.),(1.,0.848395249152619,1.),(1.,0.850986216864176,1.),(1.,0.855606962686709,
1.),(1.,0.857636888703722,1.),(1.,0.8602278199237,1.),(1.,0.861017295679405,
1.),(1.,0.862419224745804,1.),(1.,0.863034322359246,1.),(1.,0.865683471685309,
1.),(1.,0.866451432203406,1.),(1.,0.865641730003829,1.),(1.,0.865389467353775,
1.),(1.,0.864714302219193,1.),(1.,0.864291039129234,1.),(1.,0.86277153604855,
1.),(1.,0.861426213021591,1.),(1.,0.858926691433344,1.),(1.,0.858013099107921,
1.),(1.,0.856026014492253,1.),(1.,0.854948935558772,1.),(1.,0.851506192238033,
1.),(1.,0.848937517425913,1.),(1.,0.843296974763785,1.),(1.,0.840224952153864,
1.),(1.,0.8336016201822,1.),(1.,0.830031077299088,1.),(1.,0.818809152212393,
1.),(1.,0.81063662127041,1.),(1.,0.797446978165214,1.),(1.,0.79287294175514,
1.),(1.,0.783536949391413,1.),(1.,0.778775433925223,1.),(1.,0.764221056564304,
1.),(1.,0.754161223208502,1.),(1.,0.741128124491506,1.),(1.,0.738495960101228,
1.),(1.,0.733227832409877,1.),(1.,0.73058673990845,1.),(1.,0.722641688562826,
1.),(1.,0.717316009840618,1.),(1.,0.701244534517407,1.),(1.,0.69040523908201,
1.),(1.,0.676661477613371,1.),(1.,0.673899376379567,1.),(1.,0.668400924686399,
1.),(1.,0.665659348664101,1.),(1.,0.657456353546401,1.),(1.,0.652016628878085,
1.),(1.,0.646603422936515,1.)))
REPRESENTATION_ITEM('')
SURFACE()
);
#17=(
BOUNDED_SURFACE()
B_SPLINE_SURFACE(3,2,((#17883,#17884,#17885),(#17886,#17887,#17888),(#17889,
#17890,#17891),(#17892,#17893,#17894),(#17895,#17896,#17897),(#17898,#17899,
#17900),(#17901,#17902,#17903),(#17904,#17905,#17906),(#17907,#17908,#17909),
(#17910,#17911,#17912),(#17913,#17914,#17915),(#17916,#17917,#17918),(#17919,
#17920,#17921),(#17922,#17923,#17924),(#17925,#17926,#17927),(#17928,#17929,
#17930),(#17931,#17932,#17933),(#17934,#17935,#17936),(#17937,#17938,#17939),
(#17940,#17941,#17942),(#17943,#17944,#17945),(#17946,#17947,#17948),(#17949,
#17950,#17951),(#17952,#17953,#17954),(#17955,#17956,#17957),(#17958,#17959,
#17960),(#17961,#17962,#17963),(#17964,#17965,#17966),(#17967,#17968,#17969),
(#17970,#17971,#17972),(#17973,#17974,#17975),(#17976,#17977,#17978),(#17979,
#17980,#17981),(#17982,#17983,#17984),(#17985,#17986,#17987),(#17988,#17989,
#17990),(#17991,#17992,#17993),(#17994,#17995,#17996),(#17997,#17998,#17999),
(#18000,#18001,#18002),(#18003,#18004,#18005),(#18006,#18007,#18008),(#18009,
#18010,#18011),(#18012,#18013,#18014),(#18015,#18016,#18017),(#18018,#18019,
#18020),(#18021,#18022,#18023),(#18024,#18025,#18026),(#18027,#18028,#18029),
(#18030,#18031,#18032),(#18033,#18034,#18035),(#18036,#18037,#18038),(#18039,
#18040,#18041),(#18042,#18043,#18044),(#18045,#18046,#18047),(#18048,#18049,
#18050),(#18051,#18052,#18053),(#18054,#18055,#18056)),.UNSPECIFIED.,.F.,
 .F.,.F.)
B_SPLINE_SURFACE_WITH_KNOTS((4,2,2,2,2,2,2,2,2,2,2,2,2,2,2,2,2,2,2,2,2,
2,2,2,2,2,2,2,4),(3,3),(0.00822791099999177,0.0087421553258349,0.00899927754130063,
0.00925639975676637,0.0095135219722321,0.00964208307996496,0.00977064418769783,
0.0102848886186293,0.010542010834095,0.0106705719418279,0.0107991330495608,
0.0113133774804922,0.011570499695958,0.0118276219114237,0.0120847441268894,
0.0123418663423552,0.0128561107732866,0.0129846718810195,0.0131132329887524,
0.0133703552042181,0.0136274774196838,0.0137560385274167,0.0138845996351496,
0.014398844066081,0.0146559662815468,0.0149130884970125,0.015427332927944,
0.0159415773588754,0.0164558217898069),(0.,1.),.UNSPECIFIED.)
GEOMETRIC_REPRESENTATION_ITEM()
RATIONAL_B_SPLINE_SURFACE(((1.,0.646603416299739,1.),(1.,0.635777845416042,
1.),(1.,0.625055607928442,1.),(1.,0.609127621650856,1.),(1.,0.603886597603835,
1.),(1.,0.593641123894259,1.),(1.,0.588621119622324,1.),(1.,0.578794287069315,
1.),(1.,0.573987397424525,1.),(1.,0.566949594156524,1.),(1.,0.56463249225661,
1.),(1.,0.560059142358769,1.),(1.,0.557801592065279,1.),(1.,0.546803856262847,
1.),(1.,0.538816844549984,1.),(1.,0.528181154475494,1.),(1.,0.524861837914484,
1.),(1.,0.520257295698421,1.),(1.,0.518780914891841,1.),(1.,0.515996000813673,
1.),(1.,0.514683858232072,1.),(1.,0.508526013773969,1.),(1.,0.504876737837079,
1.),(1.,0.501487085264613,1.),(1.,0.500708624573569,1.),(1.,0.499919057301272,
1.),(1.,0.499897805772071,1.),(1.,0.500588074464734,1.),(1.,0.501299602522428,
1.),(1.,0.503460750293267,1.),(1.,0.504920849886908,1.),(1.,0.510276775109707,
1.),(1.,0.515155530687388,1.),(1.,0.522754639298105,1.),(1.,0.524354452613123,
1.),(1.,0.527668122842088,1.),(1.,0.529384771533702,1.),(1.,0.534705395354127,
1.),(1.,0.538479529845934,1.),(1.,0.546449215356857,1.),(1.,0.550644846474326,
1.),(1.,0.557241825447563,1.),(1.,0.559494088256871,1.),(1.,0.564052482183554,
1.),(1.,0.566363881497371,1.),(1.,0.578074130679723,1.),(1.,0.58792662900804,
1.),(1.,0.603363711869652,1.),(1.,0.608631647710062,1.),(1.,0.619200799287702,
1.),(1.,0.624523791984873,1.),(1.,0.640605786326268,1.),(1.,0.651476203100977,
1.),(1.,0.673546440287441,1.),(1.,0.684474150861875,1.),(1.,0.706154675135167,
1.),(1.,0.716910539945856,1.),(1.,0.727605019291271,1.)))
REPRESENTATION_ITEM('')
SURFACE()
);
#18=(
BOUNDED_SURFACE()
B_SPLINE_SURFACE(3,2,((#18058,#18059,#18060),(#18061,#18062,#18063),(#18064,
#18065,#18066),(#18067,#18068,#18069),(#18070,#18071,#18072),(#18073,#18074,
#18075),(#18076,#18077,#18078),(#18079,#18080,#18081),(#18082,#18083,#18084),
(#18085,#18086,#18087),(#18088,#18089,#18090),(#18091,#18092,#18093),(#18094,
#18095,#18096),(#18097,#18098,#18099),(#18100,#18101,#18102),(#18103,#18104,
#18105),(#18106,#18107,#18108),(#18109,#18110,#18111),(#18112,#18113,#18114),
(#18115,#18116,#18117),(#18118,#18119,#18120),(#18121,#18122,#18123),(#18124,
#18125,#18126),(#18127,#18128,#18129),(#18130,#18131,#18132),(#18133,#18134,
#18135),(#18136,#18137,#18138),(#18139,#18140,#18141),(#18142,#18143,#18144),
(#18145,#18146,#18147),(#18148,#18149,#18150),(#18151,#18152,#18153),(#18154,
#18155,#18156),(#18157,#18158,#18159),(#18160,#18161,#18162),(#18163,#18164,
#18165),(#18166,#18167,#18168),(#18169,#18170,#18171),(#18172,#18173,#18174),
(#18175,#18176,#18177),(#18178,#18179,#18180),(#18181,#18182,#18183),(#18184,
#18185,#18186),(#18187,#18188,#18189),(#18190,#18191,#18192),(#18193,#18194,
#18195),(#18196,#18197,#18198),(#18199,#18200,#18201),(#18202,#18203,#18204),
(#18205,#18206,#18207),(#18208,#18209,#18210),(#18211,#18212,#18213),(#18214,
#18215,#18216),(#18217,#18218,#18219),(#18220,#18221,#18222),(#18223,#18224,
#18225),(#18226,#18227,#18228),(#18229,#18230,#18231),(#18232,#18233,#18234),
(#18235,#18236,#18237),(#18238,#18239,#18240),(#18241,#18242,#18243),(#18244,
#18245,#18246),(#18247,#18248,#18249),(#18250,#18251,#18252),(#18253,#18254,
#18255)),.UNSPECIFIED.,.F.,.F.,.F.)
B_SPLINE_SURFACE_WITH_KNOTS((4,2,2,2,2,2,2,2,2,2,2,2,2,2,2,2,2,2,2,2,2,
2,2,2,2,2,2,2,2,2,2,2,4),(3,3),(0.,0.000514244430931465,0.00102848886186293,
0.0011570499695958,0.00128561107732866,0.00154273329279439,0.00205697772372586,
0.00218553883145873,0.00231409993919159,0.00257122215465732,0.00282834437012306,
0.00295690547785592,0.00308546658558879,0.00359971101652025,0.00372827212425312,
0.00385683323198599,0.00411395544745172,0.00424251655518459,0.00437107766291745,
0.00462819987838319,0.00488532209384892,0.00514244430931465,0.00565668874024611,
0.00591381095571185,0.00617093317117758,0.00668517760210904,0.00681373870984191,
0.00694229981757478,0.00719942203304051,0.00771366646397197,0.00784222757170484,
0.00797078867943771,0.00822791089490344),(0.,1.),.UNSPECIFIED.)
GEOMETRIC_REPRESENTATION_ITEM()
RATIONAL_B_SPLINE_SURFACE(((1.,0.727605019291273,1.),(1.,0.738269745261463,
1.),(1.,0.748592075286425,1.),(1.,0.768595657332682,1.),(1.,0.778278670178458,
1.),(1.,0.78996120454496,1.),(1.,0.792280826878572,1.),(1.,0.79682842199063,
1.),(1.,0.799061536127604,1.),(1.,0.805638929370428,1.),(1.,0.809861611074089,
1.),(1.,0.822031308701317,1.),(1.,0.829487589673701,1.),(1.,0.837851454359518,
1.),(1.,0.839480856802835,1.),(1.,0.842608559784893,1.),(1.,0.84410572604416,
1.),(1.,0.848395249152509,1.),(1.,0.850986216864149,1.),(1.,0.85560696268674,
1.),(1.,0.857636888703671,1.),(1.,0.860227819923728,1.),(1.,0.861017295679411,
1.),(1.,0.862419224745796,1.),(1.,0.863034322359203,1.),(1.,0.865683471685481,
1.),(1.,0.86645143220361,1.),(1.,0.865641730003779,1.),(1.,0.865389467353773,
1.),(1.,0.864714302219195,1.),(1.,0.864291039129257,1.),(1.,0.862771536048502,
1.),(1.,0.861426213021595,1.),(1.,0.858926691433342,1.),(1.,0.858013099107929,
1.),(1.,0.856026014492242,1.),(1.,0.854948935558757,1.),(1.,0.851506192238061,
1.),(1.,0.848937517425937,1.),(1.,0.84329697476376,1.),(1.,0.84022495215382,
1.),(1.,0.833601620182241,1.),(1.,0.830031077299101,1.),(1.,0.818809152212363,
1.),(1.,0.810636621270581,1.),(1.,0.797446978165125,1.),(1.,0.792872941755087,
1.),(1.,0.783536949391466,1.),(1.,0.778775433925213,1.),(1.,0.764221056564323,
1.),(1.,0.754161223208549,1.),(1.,0.741128124491493,1.),(1.,0.738495960101291,
1.),(1.,0.73322783240981,1.),(1.,0.73058673990848,1.),(1.,0.722641688562763,
1.),(1.,0.717316009840587,1.),(1.,0.701244534517476,1.),(1.,0.690405239082108,
1.),(1.,0.676661477613348,1.),(1.,0.673899376379507,1.),(1.,0.66840092468646,
1.),(1.,0.665659348664103,1.),(1.,0.657456353546395,1.),(1.,0.652016628878089,
1.),(1.,0.646603422936514,1.)))
REPRESENTATION_ITEM('')
SURFACE()
);
#19=(
BOUNDED_SURFACE()
B_SPLINE_SURFACE(3,2,((#18258,#18259,#18260),(#18261,#18262,#18263),(#18264,
#18265,#18266),(#18267,#18268,#18269),(#18270,#18271,#18272),(#18273,#18274,
#18275),(#18276,#18277,#18278),(#18279,#18280,#18281),(#18282,#18283,#18284),
(#18285,#18286,#18287),(#18288,#18289,#18290),(#18291,#18292,#18293),(#18294,
#18295,#18296),(#18297,#18298,#18299),(#18300,#18301,#18302),(#18303,#18304,
#18305),(#18306,#18307,#18308),(#18309,#18310,#18311),(#18312,#18313,#18314),
(#18315,#18316,#18317),(#18318,#18319,#18320),(#18321,#18322,#18323),(#18324,
#18325,#18326),(#18327,#18328,#18329),(#18330,#18331,#18332),(#18333,#18334,
#18335),(#18336,#18337,#18338),(#18339,#18340,#18341),(#18342,#18343,#18344),
(#18345,#18346,#18347),(#18348,#18349,#18350),(#18351,#18352,#18353),(#18354,
#18355,#18356),(#18357,#18358,#18359),(#18360,#18361,#18362),(#18363,#18364,
#18365),(#18366,#18367,#18368),(#18369,#18370,#18371),(#18372,#18373,#18374),
(#18375,#18376,#18377),(#18378,#18379,#18380),(#18381,#18382,#18383),(#18384,
#18385,#18386),(#18387,#18388,#18389),(#18390,#18391,#18392),(#18393,#18394,
#18395),(#18396,#18397,#18398),(#18399,#18400,#18401),(#18402,#18403,#18404),
(#18405,#18406,#18407),(#18408,#18409,#18410),(#18411,#18412,#18413),(#18414,
#18415,#18416),(#18417,#18418,#18419),(#18420,#18421,#18422),(#18423,#18424,
#18425),(#18426,#18427,#18428),(#18429,#18430,#18431)),.UNSPECIFIED.,.F.,
 .F.,.F.)
B_SPLINE_SURFACE_WITH_KNOTS((4,2,2,2,2,2,2,2,2,2,2,2,2,2,2,2,2,2,2,2,2,
2,2,2,2,2,2,2,4),(3,3),(0.00822791099999177,0.0087421553258349,0.00899927754130063,
0.00925639975676636,0.0095135219722321,0.00964208307996496,0.00977064418769783,
0.0102848886186293,0.010542010834095,0.0106705719418279,0.0107991330495608,
0.0113133774804922,0.011570499695958,0.0118276219114237,0.0120847441268894,
0.0123418663423552,0.0128561107732866,0.0129846718810195,0.0131132329887524,
0.0133703552042181,0.0136274774196838,0.0137560385274167,0.0138845996351495,
0.014398844066081,0.0146559662815467,0.0149130884970125,0.0154273329279439,
0.0159415773588754,0.0164558217898069),(0.,1.),.UNSPECIFIED.)
GEOMETRIC_REPRESENTATION_ITEM()
RATIONAL_B_SPLINE_SURFACE(((1.,0.646603416299739,1.),(1.,0.635777845415872,
1.),(1.,0.625055607928666,1.),(1.,0.609127621650746,1.),(1.,0.603886597603766,
1.),(1.,0.593641123894325,1.),(1.,0.588621119622213,1.),(1.,0.578794287069424,
1.),(1.,0.573987397424613,1.),(1.,0.566949594156483,1.),(1.,0.564632492256567,
1.),(1.,0.560059142358813,1.),(1.,0.557801592065364,1.),(1.,0.546803856262498,
1.),(1.,0.538816844550381,1.),(1.,0.528181154475289,1.),(1.,0.524861837914536,
1.),(1.,0.520257295698394,1.),(1.,0.518780914891774,1.),(1.,0.515996000813732,
1.),(1.,0.514683858232152,1.),(1.,0.508526013773653,1.),(1.,0.504876737837329,
1.),(1.,0.501487085264488,1.),(1.,0.500708624573413,1.),(1.,0.499919057301424,
1.),(1.,0.499897805772289,1.),(1.,0.500588074464511,1.),(1.,0.501299602522455,
1.),(1.,0.503460750293236,1.),(1.,0.504920849887092,1.),(1.,0.510276775109342,
1.),(1.,0.515155530687803,1.),(1.,0.522754639298001,1.),(1.,0.52435445261312,
1.),(1.,0.527668122842095,1.),(1.,0.529384771533763,1.),(1.,0.534705395354007,
1.),(1.,0.538479529845905,1.),(1.,0.546449215356886,1.),(1.,0.550644846474304,
1.),(1.,0.55724182544757,1.),(1.,0.559494088256935,1.),(1.,0.564052482183492,
1.),(1.,0.566363881497433,1.),(1.,0.578074130679462,1.),(1.,0.587926629008058,
1.),(1.,0.603363711869641,1.),(1.,0.608631647710066,1.),(1.,0.619200799287697,
1.),(1.,0.624523791984965,1.),(1.,0.640605786326088,1.),(1.,0.651476203100892,
1.),(1.,0.67354644028753,1.),(1.,0.684474150861655,1.),(1.,0.706154675135388,
1.),(1.,0.716910539945691,1.),(1.,0.727605019291273,1.)))
REPRESENTATION_ITEM('')
SURFACE()
);
#20=(
BOUNDED_SURFACE()
B_SPLINE_SURFACE(3,2,((#18433,#18434,#18435),(#18436,#18437,#18438),(#18439,
#18440,#18441),(#18442,#18443,#18444),(#18445,#18446,#18447),(#18448,#18449,
#18450),(#18451,#18452,#18453),(#18454,#18455,#18456),(#18457,#18458,#18459),
(#18460,#18461,#18462),(#18463,#18464,#18465),(#18466,#18467,#18468),(#18469,
#18470,#18471),(#18472,#18473,#18474),(#18475,#18476,#18477),(#18478,#18479,
#18480),(#18481,#18482,#18483),(#18484,#18485,#18486),(#18487,#18488,#18489),
(#18490,#18491,#18492),(#18493,#18494,#18495),(#18496,#18497,#18498),(#18499,
#18500,#18501),(#18502,#18503,#18504),(#18505,#18506,#18507),(#18508,#18509,
#18510),(#18511,#18512,#18513),(#18514,#18515,#18516),(#18517,#18518,#18519),
(#18520,#18521,#18522),(#18523,#18524,#18525),(#18526,#18527,#18528),(#18529,
#18530,#18531),(#18532,#18533,#18534),(#18535,#18536,#18537),(#18538,#18539,
#18540),(#18541,#18542,#18543),(#18544,#18545,#18546),(#18547,#18548,#18549),
(#18550,#18551,#18552),(#18553,#18554,#18555),(#18556,#18557,#18558),(#18559,
#18560,#18561),(#18562,#18563,#18564),(#18565,#18566,#18567),(#18568,#18569,
#18570),(#18571,#18572,#18573),(#18574,#18575,#18576),(#18577,#18578,#18579),
(#18580,#18581,#18582),(#18583,#18584,#18585),(#18586,#18587,#18588),(#18589,
#18590,#18591),(#18592,#18593,#18594),(#18595,#18596,#18597),(#18598,#18599,
#18600),(#18601,#18602,#18603),(#18604,#18605,#18606),(#18607,#18608,#18609),
(#18610,#18611,#18612),(#18613,#18614,#18615),(#18616,#18617,#18618),(#18619,
#18620,#18621),(#18622,#18623,#18624),(#18625,#18626,#18627),(#18628,#18629,
#18630)),.UNSPECIFIED.,.F.,.F.,.F.)
B_SPLINE_SURFACE_WITH_KNOTS((4,2,2,2,2,2,2,2,2,2,2,2,2,2,2,2,2,2,2,2,2,
2,2,2,2,2,2,2,2,2,2,2,4),(3,3),(0.,0.000514244430931465,0.00102848886186293,
0.0011570499695958,0.00128561107732866,0.00154273329279439,0.00205697772372586,
0.00218553883145872,0.00231409993919159,0.00257122215465732,0.00282834437012306,
0.00295690547785592,0.00308546658558879,0.00359971101652025,0.00372827212425312,
0.00385683323198598,0.00411395544745172,0.00424251655518458,0.00437107766291745,
0.00462819987838318,0.00488532209384891,0.00514244430931465,0.00565668874024611,
0.00591381095571184,0.00617093317117758,0.00668517760210904,0.00681373870984191,
0.00694229981757477,0.0071994220330405,0.00771366646397197,0.00784222757170484,
0.0079707886794377,0.00822791089490343),(0.,1.),.UNSPECIFIED.)
GEOMETRIC_REPRESENTATION_ITEM()
RATIONAL_B_SPLINE_SURFACE(((1.,0.727605019291272,1.),(1.,0.738269745261418,
1.),(1.,0.748592075286484,1.),(1.,0.768595657332627,1.),(1.,0.778278670178632,
1.),(1.,0.789961204544917,1.),(1.,0.792280826878605,1.),(1.,0.7968284219906,
1.),(1.,0.79906153612763,1.),(1.,0.805638929370375,1.),(1.,0.809861611074038,
1.),(1.,0.822031308701422,1.),(1.,0.829487589673633,1.),(1.,0.837851454359535,
1.),(1.,0.839480856802865,1.),(1.,0.842608559784865,1.),(1.,0.844105726044142,
1.),(1.,0.848395249152548,1.),(1.,0.850986216864158,1.),(1.,0.855606962686729,
1.),(1.,0.857636888703733,1.),(1.,0.860227819923696,1.),(1.,0.861017295679429,
1.),(1.,0.862419224745775,1.),(1.,0.863034322359217,1.),(1.,0.865683471685423,
1.),(1.,0.8664514322036,1.),(1.,0.865641730003782,1.),(1.,0.865389467353701,
1.),(1.,0.864714302219268,1.),(1.,0.864291039129274,1.),(1.,0.862771536048468,
1.),(1.,0.861426213021662,1.),(1.,0.858926691433307,1.),(1.,0.858013099107948,
1.),(1.,0.856026014492222,1.),(1.,0.854948935558751,1.),(1.,0.851506192238077,
1.),(1.,0.848937517425951,1.),(1.,0.843296974763746,1.),(1.,0.840224952153844,
1.),(1.,0.833601620182217,1.),(1.,0.830031077299082,1.),(1.,0.818809152212401,
1.),(1.,0.810636621270399,1.),(1.,0.797446978165217,1.),(1.,0.792872941755192,
1.),(1.,0.78353694939136,1.),(1.,0.778775433925171,1.),(1.,0.76422105656441,
1.),(1.,0.754161223208599,1.),(1.,0.741128124491482,1.),(1.,0.738495960101249,
1.),(1.,0.733227832409854,1.),(1.,0.730586739908469,1.),(1.,0.722641688562787,
1.),(1.,0.717316009840657,1.),(1.,0.701244534517331,1.),(1.,0.69040523908203,
1.),(1.,0.676661477613367,1.),(1.,0.673899376379489,1.),(1.,0.668400924686475,
1.),(1.,0.665659348664065,1.),(1.,0.657456353546472,1.),(1.,0.652016628878031,
1.),(1.,0.646603422936515,1.)))
REPRESENTATION_ITEM('')
SURFACE()
);
#21=(
BOUNDED_SURFACE()
B_SPLINE_SURFACE(3,2,((#18633,#18634,#18635),(#18636,#18637,#18638),(#18639,
#18640,#18641),(#18642,#18643,#18644),(#18645,#18646,#18647),(#18648,#18649,
#18650),(#18651,#18652,#18653),(#18654,#18655,#18656),(#18657,#18658,#18659),
(#18660,#18661,#18662),(#18663,#18664,#18665),(#18666,#18667,#18668),(#18669,
#18670,#18671),(#18672,#18673,#18674),(#18675,#18676,#18677),(#18678,#18679,
#18680),(#18681,#18682,#18683),(#18684,#18685,#18686),(#18687,#18688,#18689),
(#18690,#18691,#18692),(#18693,#18694,#18695),(#18696,#18697,#18698),(#18699,
#18700,#18701),(#18702,#18703,#18704),(#18705,#18706,#18707),(#18708,#18709,
#18710),(#18711,#18712,#18713),(#18714,#18715,#18716),(#18717,#18718,#18719),
(#18720,#18721,#18722),(#18723,#18724,#18725),(#18726,#18727,#18728),(#18729,
#18730,#18731),(#18732,#18733,#18734),(#18735,#18736,#18737),(#18738,#18739,
#18740),(#18741,#18742,#18743),(#18744,#18745,#18746),(#18747,#18748,#18749),
(#18750,#18751,#18752),(#18753,#18754,#18755),(#18756,#18757,#18758),(#18759,
#18760,#18761),(#18762,#18763,#18764),(#18765,#18766,#18767),(#18768,#18769,
#18770),(#18771,#18772,#18773),(#18774,#18775,#18776),(#18777,#18778,#18779),
(#18780,#18781,#18782),(#18783,#18784,#18785),(#18786,#18787,#18788),(#18789,
#18790,#18791),(#18792,#18793,#18794),(#18795,#18796,#18797),(#18798,#18799,
#18800),(#18801,#18802,#18803),(#18804,#18805,#18806)),.UNSPECIFIED.,.F.,
 .F.,.F.)
B_SPLINE_SURFACE_WITH_KNOTS((4,2,2,2,2,2,2,2,2,2,2,2,2,2,2,2,2,2,2,2,2,
2,2,2,2,2,2,2,4),(3,3),(0.00822791099999177,0.00874215532583489,0.00899927754130062,
0.00925639975676636,0.00951352197223209,0.00964208307996495,0.00977064418769782,
0.0102848886186293,0.010542010834095,0.0106705719418279,0.0107991330495608,
0.0113133774804922,0.0115704996959579,0.0118276219114237,0.0120847441268894,
0.0123418663423551,0.0128561107732866,0.0129846718810195,0.0131132329887523,
0.0133703552042181,0.0136274774196838,0.0137560385274167,0.0138845996351495,
0.014398844066081,0.0146559662815467,0.0149130884970125,0.0154273329279439,
0.0159415773588754,0.0164558217898069),(0.,1.),.UNSPECIFIED.)
GEOMETRIC_REPRESENTATION_ITEM()
RATIONAL_B_SPLINE_SURFACE(((1.,0.64660341629974,1.),(1.,0.635777845416019,
1.),(1.,0.625055607928472,1.),(1.,0.609127621650842,1.),(1.,0.603886597603866,
1.),(1.,0.593641123894224,1.),(1.,0.588621119622273,1.),(1.,0.57879428706936,
1.),(1.,0.573987397424623,1.),(1.,0.566949594156479,1.),(1.,0.564632492256641,
1.),(1.,0.560059142358733,1.),(1.,0.557801592065363,1.),(1.,0.546803856262522,
1.),(1.,0.538816844550033,1.),(1.,0.52818115447547,1.),(1.,0.524861837914559,
1.),(1.,0.52025729569838,1.),(1.,0.518780914891759,1.),(1.,0.515996000813751,
1.),(1.,0.514683858231971,1.),(1.,0.508526013774383,1.),(1.,0.504876737837149,
1.),(1.,0.501487085264582,1.),(1.,0.500708624573323,1.),(1.,0.499919057301517,
1.),(1.,0.499897805772192,1.),(1.,0.500588074464606,1.),(1.,0.501299602522453,
1.),(1.,0.503460750293243,1.),(1.,0.504920849886778,1.),(1.,0.510276775109967,
1.),(1.,0.51515553068733,1.),(1.,0.52275463929812,1.),(1.,0.524354452613149,
1.),(1.,0.527668122842061,1.),(1.,0.529384771533734,1.),(1.,0.53470539535405,
1.),(1.,0.538479529845885,1.),(1.,0.546449215356904,1.),(1.,0.550644846474257,
1.),(1.,0.557241825447595,1.),(1.,0.559494088257005,1.),(1.,0.564052482183427,
1.),(1.,0.566363881497423,1.),(1.,0.578074130679511,1.),(1.,0.587926629007972,
1.),(1.,0.603363711869685,1.),(1.,0.608631647710115,1.),(1.,0.619200799287649,
1.),(1.,0.624523791984868,1.),(1.,0.640605786326278,1.),(1.,0.651476203100764,
1.),(1.,0.673546440287654,1.),(1.,0.684474150861837,1.),(1.,0.706154675135206,
1.),(1.,0.716910539945826,1.),(1.,0.727605019291272,1.)))
REPRESENTATION_ITEM('')
SURFACE()
);
#22=SPHERICAL_SURFACE('',#9159,0.000300000000137179);
#23=CONICAL_SURFACE('',#8568,0.,0.78539816339745);
#24=CONICAL_SURFACE('',#8604,0.,0.78539816339745);
#25=CONICAL_SURFACE('',#8779,0.,0.244978663126864);
#26=CONICAL_SURFACE('',#8826,0.,0.244978663126864);
#27=CONICAL_SURFACE('',#8832,0.,0.523598775627269);
#28=CONICAL_SURFACE('',#9139,0.,1.04719755119693);
#29=CONICAL_SURFACE('',#9140,0.,1.04719755119693);
#30=CONICAL_SURFACE('',#9143,0.,1.04719755119693);
#31=CONICAL_SURFACE('',#9144,0.,1.04719755119693);
#32=CONICAL_SURFACE('',#9145,0.,1.04719755119693);
#33=CONICAL_SURFACE('',#9146,0.,1.04719755119693);
#34=TOROIDAL_SURFACE('',#8549,0.00799999999990077,0.000500000000345792);
#35=TOROIDAL_SURFACE('',#8551,0.0119999999999008,0.000500000000345788);
#36=TOROIDAL_SURFACE('',#8555,0.00799999999990077,0.00050000000034579);
#37=TOROIDAL_SURFACE('',#8561,0.00950000000009923,0.000500000000345799);
#38=TOROIDAL_SURFACE('',#8563,0.00849999999905548,0.000499999999472932);
#39=TOROIDAL_SURFACE('',#8564,0.00849999999905548,0.000499999999472929);
#40=TOROIDAL_SURFACE('',#8570,0.00799999999935485,0.00100000000059717);
#41=TOROIDAL_SURFACE('',#8572,0.00799999999935485,0.00100000000059717);
#42=TOROIDAL_SURFACE('',#8573,0.00800000000094452,0.000499999999472942);
#43=TOROIDAL_SURFACE('',#8574,0.00800000000094452,0.000499999999472943);
#44=TOROIDAL_SURFACE('',#8585,0.00799999999990077,0.000500000000345792);
#45=TOROIDAL_SURFACE('',#8587,0.0109999999999008,0.00050000000034579);
#46=TOROIDAL_SURFACE('',#8591,0.00799999999990077,0.00050000000034579);
#47=TOROIDAL_SURFACE('',#8597,0.00950000000009923,0.000500000000345799);
#48=TOROIDAL_SURFACE('',#8599,0.00849999999905548,0.000499999999472932);
#49=TOROIDAL_SURFACE('',#8600,0.00849999999905548,0.000499999999472929);
#50=TOROIDAL_SURFACE('',#8606,0.00799999999935485,0.00100000000059717);
#51=TOROIDAL_SURFACE('',#8608,0.00799999999935485,0.00100000000059717);
#52=TOROIDAL_SURFACE('',#8609,0.00800000000094452,0.000499999999472942);
#53=TOROIDAL_SURFACE('',#8610,0.00800000000094452,0.000499999999472943);
#54=TOROIDAL_SURFACE('',#8614,0.0117000000001705,0.000300000000224998);
#55=TOROIDAL_SURFACE('',#8623,0.0117000000001705,0.000300000000224998);
#56=TOROIDAL_SURFACE('',#8625,0.00974999999980933,0.00134999999974855);
#57=TOROIDAL_SURFACE('',#8626,0.00974999999980933,0.00134999999974855);
#58=TOROIDAL_SURFACE('',#8637,0.00975000000019067,0.00134999999974855);
#59=TOROIDAL_SURFACE('',#8638,0.00975000000019067,0.00134999999974855);
#60=TOROIDAL_SURFACE('',#8640,0.00779999999982954,0.000300000000224997);
#61=TOROIDAL_SURFACE('',#8641,0.00779999999982954,0.000300000000224997);
#62=TOROIDAL_SURFACE('',#8650,0.00779999999982955,0.000300000000225003);
#63=TOROIDAL_SURFACE('',#8651,0.00779999999982955,0.000300000000225003);
#64=TOROIDAL_SURFACE('',#8653,0.0117000000001705,0.000300000000224998);
#65=TOROIDAL_SURFACE('',#8662,0.0117000000001705,0.000300000000224998);
#66=TOROIDAL_SURFACE('',#8664,0.00974999999980933,0.00134999999974855);
#67=TOROIDAL_SURFACE('',#8665,0.00974999999980933,0.00134999999974855);
#68=TOROIDAL_SURFACE('',#8676,0.00975000000019067,0.00134999999974855);
#69=TOROIDAL_SURFACE('',#8677,0.00975000000019067,0.00134999999974855);
#70=TOROIDAL_SURFACE('',#8679,0.00779999999982954,0.000300000000224997);
#71=TOROIDAL_SURFACE('',#8680,0.00779999999982954,0.000300000000224997);
#72=TOROIDAL_SURFACE('',#8689,0.00779999999982955,0.000300000000225003);
#73=TOROIDAL_SURFACE('',#8690,0.00779999999982955,0.000300000000225003);
#74=TOROIDAL_SURFACE('',#8817,0.0329999999999897,0.000999999999849241);
#75=TOROIDAL_SURFACE('',#8829,0.0329999999999897,0.000999999999849247);
#76=TOROIDAL_SURFACE('',#8836,0.0180358983802304,0.0019999999955971);
#77=TOROIDAL_SURFACE('',#8838,0.0180358983802304,0.00199999999559711);
#78=TOROIDAL_SURFACE('',#8844,0.0127999999998295,0.000300000000224998);
#79=TOROIDAL_SURFACE('',#8846,0.0175358983901566,0.00149999999951453);
#80=TOROIDAL_SURFACE('',#8849,0.0175358983836069,0.0015000000001222);
#81=TOROIDAL_SURFACE('',#8852,0.0175358984068633,0.00150000000032502);
#82=TOROIDAL_SURFACE('',#8854,0.017535898384194,0.00149999999953639);
#83=TOROIDAL_SURFACE('',#8857,0.0175358984068637,0.001500000000325);
#84=TOROIDAL_SURFACE('',#8859,0.0175358983836068,0.0015000000001222);
#85=TOROIDAL_SURFACE('',#8862,0.0175358983793295,0.00149999999977719);
#86=TOROIDAL_SURFACE('',#8864,0.0175358983793296,0.00149999999977719);
#87=TOROIDAL_SURFACE('',#8866,0.0175358983836071,0.0015000000001222);
#88=TOROIDAL_SURFACE('',#8869,0.0175358984068636,0.00150000000032501);
#89=TOROIDAL_SURFACE('',#8871,0.0175358983841942,0.00149999999953638);
#90=TOROIDAL_SURFACE('',#8874,0.0175358984068633,0.00150000000032502);
#91=TOROIDAL_SURFACE('',#8876,0.017535898383607,0.0015000000001222);
#92=TOROIDAL_SURFACE('',#8967,0.0157358983846276,0.000299999999947084);
#93=TOROIDAL_SURFACE('',#9056,0.0329999999999897,0.000999999999849243);
#94=TOROIDAL_SURFACE('',#9060,0.0163358983848296,0.000300000000224998);
#95=TOROIDAL_SURFACE('',#9062,0.0329999999999897,0.000999999999849251);
#96=TOROIDAL_SURFACE('',#9065,0.0163358983848296,0.000300000000224997);
#97=TOROIDAL_SURFACE('',#9090,0.0175358983853182,0.00150000000045805);
#98=TOROIDAL_SURFACE('',#9094,0.0175358983853182,0.00150000000045805);
#99=TOROIDAL_SURFACE('',#9095,0.0024500000000844,0.000300000000050416);
#100=TOROIDAL_SURFACE('',#9097,0.00244999999982957,0.000300000000225024);
#101=TOROIDAL_SURFACE('',#9099,0.00244999999982957,0.000300000000225024);
#102=TOROIDAL_SURFACE('',#9100,0.00245000000008441,0.000300000000050426);
#103=TOROIDAL_SURFACE('',#9103,0.00245000000008441,0.000300000000050429);
#104=TOROIDAL_SURFACE('',#9106,0.00244999999982957,0.000300000000225019);
#105=TOROIDAL_SURFACE('',#9108,0.00244999999982957,0.000300000000225023);
#106=TOROIDAL_SURFACE('',#9110,0.0024500000000844,0.000300000000050417);
#107=TOROIDAL_SURFACE('',#9113,0.0236999999712056,0.000299999999854375);
#108=TOROIDAL_SURFACE('',#9117,0.0236999999712051,0.000299999999854371);
#109=TOROIDAL_SURFACE('',#9122,0.0236999999559749,0.000300000000142203);
#110=TOROIDAL_SURFACE('',#9128,0.0236999999712049,0.00029999999985436);
#111=TOROIDAL_SURFACE('',#9132,0.0236999999712049,0.000299999999854394);
#112=TOROIDAL_SURFACE('',#9136,0.0236999999850598,0.000300000000477842);
#113=TOROIDAL_SURFACE('',#9174,0.0236999999761744,0.000300000000837741);
#114=TOROIDAL_SURFACE('',#9177,0.0236999999817642,0.000300000000595368);
#115=TOROIDAL_SURFACE('',#9181,0.0236999999761741,0.000300000000837734);
#116=TOROIDAL_SURFACE('',#9184,0.0236999999761741,0.000300000000837742);
#117=TOROIDAL_SURFACE('',#9187,0.0236999999817642,0.000300000000595372);
#118=TOROIDAL_SURFACE('',#9190,0.023699999976173,0.000300000000837742);
#119=CONTEXT_DEPENDENT_SHAPE_REPRESENTATION(#131,#18829);
#120=CONTEXT_DEPENDENT_SHAPE_REPRESENTATION(#132,#18831);
#121=CONTEXT_DEPENDENT_SHAPE_REPRESENTATION(#133,#18833);
#122=CONTEXT_DEPENDENT_SHAPE_REPRESENTATION(#134,#18835);
#123=CONTEXT_DEPENDENT_SHAPE_REPRESENTATION(#135,#18837);
#124=CONTEXT_DEPENDENT_SHAPE_REPRESENTATION(#136,#18839);
#125=NEXT_ASSEMBLY_USAGE_OCCURRENCE('NAUO1',
'cassette body__ DE    15749','cassette body__ DE    15749',#18840,#18841,
'');
#126=NEXT_ASSEMBLY_USAGE_OCCURRENCE('NAUO2','endcap2__ DE    22113',
'endcap2__ DE    22113',#18840,#18842,'');
#127=NEXT_ASSEMBLY_USAGE_OCCURRENCE('NAUO3','endcap__ DE    14671',
'endcap__ DE    14671',#18840,#18843,'');
#128=NEXT_ASSEMBLY_USAGE_OCCURRENCE('NAUO4',
'angular contact ball bearing_68_bsi_BS 6267 ABB - 4815 - 18,SI,NC,18_
68__ DE    23193',
'angular contact ball bearing_68_bsi_BS 6267 ABB - 4815 - 18,SI,NC,18_
68__ DE    23193',#18840,#18844,'');
#129=NEXT_ASSEMBLY_USAGE_OCCURRENCE('NAUO5',
'angular contact ball bearing_68_bsi_BS 6267 ABB - 4815 - 18,SI,NC,18_
68__ DE    23193',
'angular contact ball bearing_68_bsi_BS 6267 ABB - 4815 - 18,SI,NC,18_
68__ DE    23193',#18840,#18845,'');
#130=NEXT_ASSEMBLY_USAGE_OCCURRENCE('NAUO6','HubBody__ DE       35',
'HubBody__ DE       35',#18840,#18846,'');
#131=(
REPRESENTATION_RELATIONSHIP(' ',' ',#8233,#8232)
REPRESENTATION_RELATIONSHIP_WITH_TRANSFORMATION(#137)
SHAPE_REPRESENTATION_RELATIONSHIP()
);
#132=(
REPRESENTATION_RELATIONSHIP(' ',' ',#8234,#8232)
REPRESENTATION_RELATIONSHIP_WITH_TRANSFORMATION(#138)
SHAPE_REPRESENTATION_RELATIONSHIP()
);
#133=(
REPRESENTATION_RELATIONSHIP(' ',' ',#8235,#8232)
REPRESENTATION_RELATIONSHIP_WITH_TRANSFORMATION(#139)
SHAPE_REPRESENTATION_RELATIONSHIP()
);
#134=(
REPRESENTATION_RELATIONSHIP(' ',' ',#8236,#8232)
REPRESENTATION_RELATIONSHIP_WITH_TRANSFORMATION(#140)
SHAPE_REPRESENTATION_RELATIONSHIP()
);
#135=(
REPRESENTATION_RELATIONSHIP(' ',' ',#8237,#8232)
REPRESENTATION_RELATIONSHIP_WITH_TRANSFORMATION(#141)
SHAPE_REPRESENTATION_RELATIONSHIP()
);
#136=(
REPRESENTATION_RELATIONSHIP(' ',' ',#8238,#8232)
REPRESENTATION_RELATIONSHIP_WITH_TRANSFORMATION(#142)
SHAPE_REPRESENTATION_RELATIONSHIP()
);
#137=ITEM_DEFINED_TRANSFORMATION(' ',' ',#8239,#8541);
#138=ITEM_DEFINED_TRANSFORMATION(' ',' ',#8239,#8577);
#139=ITEM_DEFINED_TRANSFORMATION(' ',' ',#8239,#8613);
#140=ITEM_DEFINED_TRANSFORMATION(' ',' ',#8239,#8652);
#141=ITEM_DEFINED_TRANSFORMATION(' ',' ',#8239,#8691);
#142=ITEM_DEFINED_TRANSFORMATION(' ',' ',#8239,#9191);
#143=SHAPE_REPRESENTATION_RELATIONSHIP('','',#8233,#149);
#144=SHAPE_REPRESENTATION_RELATIONSHIP('','',#8234,#150);
#145=SHAPE_REPRESENTATION_RELATIONSHIP('','',#8235,#151);
#146=SHAPE_REPRESENTATION_RELATIONSHIP('','',#8236,#152);
#147=SHAPE_REPRESENTATION_RELATIONSHIP('','',#8237,#153);
#148=SHAPE_REPRESENTATION_RELATIONSHIP('','',#8238,#154);
#149=ADVANCED_BREP_SHAPE_REPRESENTATION('',(#8219),#18811);
#150=ADVANCED_BREP_SHAPE_REPRESENTATION('',(#8220),#18812);
#151=ADVANCED_BREP_SHAPE_REPRESENTATION('',(#8221),#18813);
#152=ADVANCED_BREP_SHAPE_REPRESENTATION('',(#8222),#18814);
#153=ADVANCED_BREP_SHAPE_REPRESENTATION('',(#8223),#18815);
#154=ADVANCED_BREP_SHAPE_REPRESENTATION('',(#8224),#18816);
#155=B_SPLINE_CURVE_WITH_KNOTS('',3,(#11114,#11115,#11116,#11117),
 .UNSPECIFIED.,.F.,.F.,(4,4),(0.,1.),.UNSPECIFIED.);
#156=B_SPLINE_CURVE_WITH_KNOTS('',3,(#11121,#11122,#11123,#11124),
 .UNSPECIFIED.,.F.,.F.,(4,4),(0.,1.),.UNSPECIFIED.);
#157=B_SPLINE_CURVE_WITH_KNOTS('',3,(#11128,#11129,#11130,#11131),
 .UNSPECIFIED.,.F.,.F.,(4,4),(0.,1.),.UNSPECIFIED.);
#158=B_SPLINE_CURVE_WITH_KNOTS('',3,(#11135,#11136,#11137,#11138),
 .UNSPECIFIED.,.F.,.F.,(4,4),(0.,1.),.UNSPECIFIED.);
#159=B_SPLINE_CURVE_WITH_KNOTS('',3,(#11142,#11143,#11144,#11145),
 .UNSPECIFIED.,.F.,.F.,(4,4),(0.,1.),.UNSPECIFIED.);
#160=B_SPLINE_CURVE_WITH_KNOTS('',3,(#11149,#11150,#11151,#11152),
 .UNSPECIFIED.,.F.,.F.,(4,4),(0.,1.),.UNSPECIFIED.);
#161=B_SPLINE_CURVE_WITH_KNOTS('',3,(#11156,#11157,#11158,#11159),
 .UNSPECIFIED.,.F.,.F.,(4,4),(0.,1.),.UNSPECIFIED.);
#162=B_SPLINE_CURVE_WITH_KNOTS('',3,(#11163,#11164,#11165,#11166),
 .UNSPECIFIED.,.F.,.F.,(4,4),(0.,1.),.UNSPECIFIED.);
#163=B_SPLINE_CURVE_WITH_KNOTS('',3,(#11170,#11171,#11172,#11173),
 .UNSPECIFIED.,.F.,.F.,(4,4),(0.,1.),.UNSPECIFIED.);
#164=B_SPLINE_CURVE_WITH_KNOTS('',3,(#11177,#11178,#11179,#11180),
 .UNSPECIFIED.,.F.,.F.,(4,4),(0.,1.),.UNSPECIFIED.);
#165=B_SPLINE_CURVE_WITH_KNOTS('',3,(#11184,#11185,#11186,#11187),
 .UNSPECIFIED.,.F.,.F.,(4,4),(0.,1.),.UNSPECIFIED.);
#166=B_SPLINE_CURVE_WITH_KNOTS('',3,(#11191,#11192,#11193,#11194),
 .UNSPECIFIED.,.F.,.F.,(4,4),(0.,1.),.UNSPECIFIED.);
#167=B_SPLINE_CURVE_WITH_KNOTS('',3,(#11198,#11199,#11200,#11201),
 .UNSPECIFIED.,.F.,.F.,(4,4),(0.,1.),.UNSPECIFIED.);
#168=B_SPLINE_CURVE_WITH_KNOTS('',3,(#11205,#11206,#11207,#11208),
 .UNSPECIFIED.,.F.,.F.,(4,4),(0.,1.),.UNSPECIFIED.);
#169=B_SPLINE_CURVE_WITH_KNOTS('',3,(#11212,#11213,#11214,#11215),
 .UNSPECIFIED.,.F.,.F.,(4,4),(0.,1.),.UNSPECIFIED.);
#170=B_SPLINE_CURVE_WITH_KNOTS('',3,(#11219,#11220,#11221,#11222),
 .UNSPECIFIED.,.F.,.F.,(4,4),(0.,1.),.UNSPECIFIED.);
#171=B_SPLINE_CURVE_WITH_KNOTS('',3,(#11226,#11227,#11228,#11229),
 .UNSPECIFIED.,.F.,.F.,(4,4),(0.,1.),.UNSPECIFIED.);
#172=B_SPLINE_CURVE_WITH_KNOTS('',3,(#11233,#11234,#11235,#11236),
 .UNSPECIFIED.,.F.,.F.,(4,4),(0.,1.),.UNSPECIFIED.);
#173=B_SPLINE_CURVE_WITH_KNOTS('',3,(#11240,#11241,#11242,#11243),
 .UNSPECIFIED.,.F.,.F.,(4,4),(0.,1.),.UNSPECIFIED.);
#174=B_SPLINE_CURVE_WITH_KNOTS('',3,(#11247,#11248,#11249,#11250),
 .UNSPECIFIED.,.F.,.F.,(4,4),(0.,1.),.UNSPECIFIED.);
#175=B_SPLINE_CURVE_WITH_KNOTS('',3,(#11254,#11255,#11256,#11257),
 .UNSPECIFIED.,.F.,.F.,(4,4),(0.,1.),.UNSPECIFIED.);
#176=B_SPLINE_CURVE_WITH_KNOTS('',3,(#11261,#11262,#11263,#11264),
 .UNSPECIFIED.,.F.,.F.,(4,4),(0.,1.),.UNSPECIFIED.);
#177=B_SPLINE_CURVE_WITH_KNOTS('',3,(#11268,#11269,#11270,#11271),
 .UNSPECIFIED.,.F.,.F.,(4,4),(0.,1.),.UNSPECIFIED.);
#178=B_SPLINE_CURVE_WITH_KNOTS('',3,(#11275,#11276,#11277,#11278),
 .UNSPECIFIED.,.F.,.F.,(4,4),(0.,1.),.UNSPECIFIED.);
#179=B_SPLINE_CURVE_WITH_KNOTS('',3,(#11282,#11283,#11284,#11285),
 .UNSPECIFIED.,.F.,.F.,(4,4),(0.,1.),.UNSPECIFIED.);
#180=B_SPLINE_CURVE_WITH_KNOTS('',3,(#11289,#11290,#11291,#11292),
 .UNSPECIFIED.,.F.,.F.,(4,4),(0.,1.),.UNSPECIFIED.);
#181=B_SPLINE_CURVE_WITH_KNOTS('',3,(#11296,#11297,#11298,#11299),
 .UNSPECIFIED.,.F.,.F.,(4,4),(0.,1.),.UNSPECIFIED.);
#182=B_SPLINE_CURVE_WITH_KNOTS('',3,(#11303,#11304,#11305,#11306),
 .UNSPECIFIED.,.F.,.F.,(4,4),(0.,1.),.UNSPECIFIED.);
#183=B_SPLINE_CURVE_WITH_KNOTS('',3,(#11310,#11311,#11312,#11313),
 .UNSPECIFIED.,.F.,.F.,(4,4),(0.,1.),.UNSPECIFIED.);
#184=B_SPLINE_CURVE_WITH_KNOTS('',3,(#11317,#11318,#11319,#11320),
 .UNSPECIFIED.,.F.,.F.,(4,4),(0.,1.),.UNSPECIFIED.);
#185=B_SPLINE_CURVE_WITH_KNOTS('',3,(#11324,#11325,#11326,#11327),
 .UNSPECIFIED.,.F.,.F.,(4,4),(0.,1.),.UNSPECIFIED.);
#186=B_SPLINE_CURVE_WITH_KNOTS('',3,(#11331,#11332,#11333,#11334),
 .UNSPECIFIED.,.F.,.F.,(4,4),(0.,1.),.UNSPECIFIED.);
#187=B_SPLINE_CURVE_WITH_KNOTS('',3,(#11338,#11339,#11340,#11341),
 .UNSPECIFIED.,.F.,.F.,(4,4),(0.,1.),.UNSPECIFIED.);
#188=B_SPLINE_CURVE_WITH_KNOTS('',3,(#11345,#11346,#11347,#11348),
 .UNSPECIFIED.,.F.,.F.,(4,4),(0.,1.),.UNSPECIFIED.);
#189=B_SPLINE_CURVE_WITH_KNOTS('',3,(#11352,#11353,#11354,#11355),
 .UNSPECIFIED.,.F.,.F.,(4,4),(0.,1.),.UNSPECIFIED.);
#190=B_SPLINE_CURVE_WITH_KNOTS('',3,(#11359,#11360,#11361,#11362),
 .UNSPECIFIED.,.F.,.F.,(4,4),(0.,1.),.UNSPECIFIED.);
#191=B_SPLINE_CURVE_WITH_KNOTS('',3,(#11366,#11367,#11368,#11369),
 .UNSPECIFIED.,.F.,.F.,(4,4),(0.,1.),.UNSPECIFIED.);
#192=B_SPLINE_CURVE_WITH_KNOTS('',3,(#11373,#11374,#11375,#11376),
 .UNSPECIFIED.,.F.,.F.,(4,4),(0.,1.),.UNSPECIFIED.);
#193=B_SPLINE_CURVE_WITH_KNOTS('',3,(#11380,#11381,#11382,#11383),
 .UNSPECIFIED.,.F.,.F.,(4,4),(0.,1.),.UNSPECIFIED.);
#194=B_SPLINE_CURVE_WITH_KNOTS('',3,(#11387,#11388,#11389,#11390),
 .UNSPECIFIED.,.F.,.F.,(4,4),(0.,1.),.UNSPECIFIED.);
#195=B_SPLINE_CURVE_WITH_KNOTS('',3,(#11395,#11396,#11397,#11398),
 .UNSPECIFIED.,.F.,.F.,(4,4),(2.69917730509592E-7,1.),.UNSPECIFIED.);
#196=B_SPLINE_CURVE_WITH_KNOTS('',3,(#11402,#11403,#11404,#11405),
 .UNSPECIFIED.,.F.,.F.,(4,4),(2.30141280936843E-7,0.999999729513626),
 .UNSPECIFIED.);
#197=B_SPLINE_CURVE_WITH_KNOTS('',3,(#11407,#11408,#11409,#11410),
 .UNSPECIFIED.,.F.,.F.,(4,4),(0.,1.),.UNSPECIFIED.);
#198=B_SPLINE_CURVE_WITH_KNOTS('',3,(#11412,#11413,#11414,#11415),
 .UNSPECIFIED.,.F.,.F.,(4,4),(0.,1.),.UNSPECIFIED.);
#199=B_SPLINE_CURVE_WITH_KNOTS('',3,(#11417,#11418,#11419,#11420),
 .UNSPECIFIED.,.F.,.F.,(4,4),(0.,1.),.UNSPECIFIED.);
#200=B_SPLINE_CURVE_WITH_KNOTS('',3,(#11425,#11426,#11427,#11428),
 .UNSPECIFIED.,.F.,.F.,(4,4),(0.,0.999999968269152),.UNSPECIFIED.);
#201=B_SPLINE_CURVE_WITH_KNOTS('',3,(#11430,#11431,#11432,#11433),
 .UNSPECIFIED.,.F.,.F.,(4,4),(2.28432714197121E-7,1.),.UNSPECIFIED.);
#202=B_SPLINE_CURVE_WITH_KNOTS('',3,(#11434,#11435,#11436,#11437),
 .UNSPECIFIED.,.F.,.F.,(4,4),(-5.00258413789748E-10,1.),.UNSPECIFIED.);
#203=B_SPLINE_CURVE_WITH_KNOTS('',3,(#11439,#11440,#11441,#11442),
 .UNSPECIFIED.,.F.,.F.,(4,4),(0.,1.),.UNSPECIFIED.);
#204=B_SPLINE_CURVE_WITH_KNOTS('',3,(#11444,#11445,#11446,#11447),
 .UNSPECIFIED.,.F.,.F.,(4,4),(0.,1.),.UNSPECIFIED.);
#205=B_SPLINE_CURVE_WITH_KNOTS('',3,(#11449,#11450,#11451,#11452),
 .UNSPECIFIED.,.F.,.F.,(4,4),(4.98889504924982E-7,1.),.UNSPECIFIED.);
#206=B_SPLINE_CURVE_WITH_KNOTS('',3,(#11456,#11457,#11458,#11459),
 .UNSPECIFIED.,.F.,.F.,(4,4),(2.30314042019811E-7,0.999999729964527),
 .UNSPECIFIED.);
#207=B_SPLINE_CURVE_WITH_KNOTS('',3,(#11461,#11462,#11463,#11464),
 .UNSPECIFIED.,.F.,.F.,(4,4),(-4.2053902482023E-16,1.),.UNSPECIFIED.);
#208=B_SPLINE_CURVE_WITH_KNOTS('',3,(#11466,#11467,#11468,#11469),
 .UNSPECIFIED.,.F.,.F.,(4,4),(0.,1.),.UNSPECIFIED.);
#209=B_SPLINE_CURVE_WITH_KNOTS('',3,(#11471,#11472,#11473,#11474),
 .UNSPECIFIED.,.F.,.F.,(4,4),(0.,1.),.UNSPECIFIED.);
#210=B_SPLINE_CURVE_WITH_KNOTS('',3,(#11476,#11477,#11478,#11479),
 .UNSPECIFIED.,.F.,.F.,(4,4),(-1.657448313855E-10,1.),.UNSPECIFIED.);
#211=B_SPLINE_CURVE_WITH_KNOTS('',3,(#11483,#11484,#11485,#11486),
 .UNSPECIFIED.,.F.,.F.,(4,4),(0.,0.999999968338702),.UNSPECIFIED.);
#212=B_SPLINE_CURVE_WITH_KNOTS('',3,(#11488,#11489,#11490,#11491),
 .UNSPECIFIED.,.F.,.F.,(4,4),(2.29200229973547E-7,1.),.UNSPECIFIED.);
#213=B_SPLINE_CURVE_WITH_KNOTS('',3,(#11493,#11494,#11495,#11496),
 .UNSPECIFIED.,.F.,.F.,(4,4),(0.,1.),.UNSPECIFIED.);
#214=B_SPLINE_CURVE_WITH_KNOTS('',3,(#11498,#11499,#11500,#11501),
 .UNSPECIFIED.,.F.,.F.,(4,4),(0.,1.),.UNSPECIFIED.);
#215=B_SPLINE_CURVE_WITH_KNOTS('',3,(#11503,#11504,#11505,#11506),
 .UNSPECIFIED.,.F.,.F.,(4,4),(4.99050153655672E-7,1.),.UNSPECIFIED.);
#216=B_SPLINE_CURVE_WITH_KNOTS('',3,(#11510,#11511,#11512,#11513),
 .UNSPECIFIED.,.F.,.F.,(4,4),(2.31126409748052E-7,0.999999730391103),
 .UNSPECIFIED.);
#217=B_SPLINE_CURVE_WITH_KNOTS('',3,(#11515,#11516,#11517,#11518),
 .UNSPECIFIED.,.F.,.F.,(4,4),(2.10269512148046E-16,1.),.UNSPECIFIED.);
#218=B_SPLINE_CURVE_WITH_KNOTS('',3,(#11520,#11521,#11522,#11523),
 .UNSPECIFIED.,.F.,.F.,(4,4),(0.,1.),.UNSPECIFIED.);
#219=B_SPLINE_CURVE_WITH_KNOTS('',3,(#11525,#11526,#11527,#11528),
 .UNSPECIFIED.,.F.,.F.,(4,4),(0.,1.),.UNSPECIFIED.);
#220=B_SPLINE_CURVE_WITH_KNOTS('',3,(#11530,#11531,#11532,#11533),
 .UNSPECIFIED.,.F.,.F.,(4,4),(-9.6786794648492E-11,1.),.UNSPECIFIED.);
#221=B_SPLINE_CURVE_WITH_KNOTS('',3,(#11537,#11538,#11539,#11540),
 .UNSPECIFIED.,.F.,.F.,(4,4),(0.,0.999999967972051),.UNSPECIFIED.);
#222=B_SPLINE_CURVE_WITH_KNOTS('',3,(#11542,#11543,#11544,#11545),
 .UNSPECIFIED.,.F.,.F.,(4,4),(2.2911260788884E-7,1.),.UNSPECIFIED.);
#223=B_SPLINE_CURVE_WITH_KNOTS('',3,(#11547,#11548,#11549,#11550),
 .UNSPECIFIED.,.F.,.F.,(4,4),(0.,1.),.UNSPECIFIED.);
#224=B_SPLINE_CURVE_WITH_KNOTS('',3,(#11552,#11553,#11554,#11555),
 .UNSPECIFIED.,.F.,.F.,(4,4),(0.,1.),.UNSPECIFIED.);
#225=B_SPLINE_CURVE_WITH_KNOTS('',3,(#11557,#11558,#11559,#11560),
 .UNSPECIFIED.,.F.,.F.,(4,4),(4.98268763671896E-7,1.),.UNSPECIFIED.);
#226=B_SPLINE_CURVE_WITH_KNOTS('',3,(#11564,#11565,#11566,#11567),
 .UNSPECIFIED.,.F.,.F.,(4,4),(2.29530257614294E-7,0.999999730208141),
 .UNSPECIFIED.);
#227=B_SPLINE_CURVE_WITH_KNOTS('',3,(#11569,#11570,#11571,#11572),
 .UNSPECIFIED.,.F.,.F.,(4,4),(-4.20539024606654E-16,1.),.UNSPECIFIED.);
#228=B_SPLINE_CURVE_WITH_KNOTS('',3,(#11574,#11575,#11576,#11577),
 .UNSPECIFIED.,.F.,.F.,(4,4),(0.,1.),.UNSPECIFIED.);
#229=B_SPLINE_CURVE_WITH_KNOTS('',3,(#11579,#11580,#11581,#11582),
 .UNSPECIFIED.,.F.,.F.,(4,4),(0.,1.),.UNSPECIFIED.);
#230=B_SPLINE_CURVE_WITH_KNOTS('',3,(#11584,#11585,#11586,#11587),
 .UNSPECIFIED.,.F.,.F.,(4,4),(-2.43327398011773E-10,1.),.UNSPECIFIED.);
#231=B_SPLINE_CURVE_WITH_KNOTS('',3,(#11591,#11592,#11593,#11594),
 .UNSPECIFIED.,.F.,.F.,(4,4),(0.,0.999999968299911),.UNSPECIFIED.);
#232=B_SPLINE_CURVE_WITH_KNOTS('',3,(#11596,#11597,#11598,#11599),
 .UNSPECIFIED.,.F.,.F.,(4,4),(2.27426734378615E-7,1.),.UNSPECIFIED.);
#233=B_SPLINE_CURVE_WITH_KNOTS('',3,(#11601,#11602,#11603,#11604),
 .UNSPECIFIED.,.F.,.F.,(4,4),(0.,1.),.UNSPECIFIED.);
#234=B_SPLINE_CURVE_WITH_KNOTS('',3,(#11606,#11607,#11608,#11609),
 .UNSPECIFIED.,.F.,.F.,(4,4),(0.,1.),.UNSPECIFIED.);
#235=B_SPLINE_CURVE_WITH_KNOTS('',3,(#11611,#11612,#11613,#11614),
 .UNSPECIFIED.,.F.,.F.,(4,4),(4.98476028789599E-7,1.),.UNSPECIFIED.);
#236=B_SPLINE_CURVE_WITH_KNOTS('',3,(#11618,#11619,#11620,#11621),
 .UNSPECIFIED.,.F.,.F.,(4,4),(2.30300781159193E-7,0.999999730293526),
 .UNSPECIFIED.);
#237=B_SPLINE_CURVE_WITH_KNOTS('',3,(#11623,#11624,#11625,#11626),
 .UNSPECIFIED.,.F.,.F.,(4,4),(6.0851059371599E-30,1.),.UNSPECIFIED.);
#238=B_SPLINE_CURVE_WITH_KNOTS('',3,(#11628,#11629,#11630,#11631),
 .UNSPECIFIED.,.F.,.F.,(4,4),(0.,1.),.UNSPECIFIED.);
#239=B_SPLINE_CURVE_WITH_KNOTS('',3,(#11633,#11634,#11635,#11636),
 .UNSPECIFIED.,.F.,.F.,(4,4),(0.,1.),.UNSPECIFIED.);
#240=B_SPLINE_CURVE_WITH_KNOTS('',3,(#11638,#11639,#11640,#11641),
 .UNSPECIFIED.,.F.,.F.,(4,4),(-2.08522840277463E-10,1.),.UNSPECIFIED.);
#241=B_SPLINE_CURVE_WITH_KNOTS('',3,(#11645,#11646,#11647,#11648),
 .UNSPECIFIED.,.F.,.F.,(4,4),(0.,0.999999968243275),.UNSPECIFIED.);
#242=B_SPLINE_CURVE_WITH_KNOTS('',3,(#11650,#11651,#11652,#11653),
 .UNSPECIFIED.,.F.,.F.,(4,4),(2.3069334227709E-7,1.),.UNSPECIFIED.);
#243=B_SPLINE_CURVE_WITH_KNOTS('',3,(#11655,#11656,#11657,#11658),
 .UNSPECIFIED.,.F.,.F.,(4,4),(0.,1.),.UNSPECIFIED.);
#244=B_SPLINE_CURVE_WITH_KNOTS('',3,(#11660,#11661,#11662,#11663),
 .UNSPECIFIED.,.F.,.F.,(4,4),(0.,1.),.UNSPECIFIED.);
#245=B_SPLINE_CURVE_WITH_KNOTS('',3,(#11665,#11666,#11667,#11668),
 .UNSPECIFIED.,.F.,.F.,(4,4),(4.9864286811645E-7,1.),.UNSPECIFIED.);
#246=B_SPLINE_CURVE_WITH_KNOTS('',3,(#11672,#11673,#11674,#11675),
 .UNSPECIFIED.,.F.,.F.,(4,4),(2.30141256725537E-7,0.999999729718004),
 .UNSPECIFIED.);
#247=B_SPLINE_CURVE_WITH_KNOTS('',3,(#11677,#11678,#11679,#11680),
 .UNSPECIFIED.,.F.,.F.,(4,4),(0.,1.),.UNSPECIFIED.);
#248=B_SPLINE_CURVE_WITH_KNOTS('',3,(#11682,#11683,#11684,#11685),
 .UNSPECIFIED.,.F.,.F.,(4,4),(0.,1.),.UNSPECIFIED.);
#249=B_SPLINE_CURVE_WITH_KNOTS('',3,(#11687,#11688,#11689,#11690),
 .UNSPECIFIED.,.F.,.F.,(4,4),(0.,1.),.UNSPECIFIED.);
#250=B_SPLINE_CURVE_WITH_KNOTS('',3,(#11692,#11693,#11694,#11695),
 .UNSPECIFIED.,.F.,.F.,(4,4),(-5.18885638844573E-10,1.),.UNSPECIFIED.);
#251=B_SPLINE_CURVE_WITH_KNOTS('',3,(#11699,#11700,#11701,#11702),
 .UNSPECIFIED.,.F.,.F.,(4,4),(0.,0.999999968088093),.UNSPECIFIED.);
#252=B_SPLINE_CURVE_WITH_KNOTS('',3,(#11704,#11705,#11706,#11707),
 .UNSPECIFIED.,.F.,.F.,(4,4),(2.28637183361211E-7,1.),.UNSPECIFIED.);
#253=B_SPLINE_CURVE_WITH_KNOTS('',3,(#11709,#11710,#11711,#11712),
 .UNSPECIFIED.,.F.,.F.,(4,4),(0.,1.),.UNSPECIFIED.);
#254=B_SPLINE_CURVE_WITH_KNOTS('',3,(#11714,#11715,#11716,#11717),
 .UNSPECIFIED.,.F.,.F.,(4,4),(0.,1.),.UNSPECIFIED.);
#255=B_SPLINE_CURVE_WITH_KNOTS('',3,(#11719,#11720,#11721,#11722),
 .UNSPECIFIED.,.F.,.F.,(4,4),(4.98889504924982E-7,1.),.UNSPECIFIED.);
#256=B_SPLINE_CURVE_WITH_KNOTS('',3,(#11726,#11727,#11728,#11729),
 .UNSPECIFIED.,.F.,.F.,(4,4),(2.3031404033356E-7,0.999999730169011),
 .UNSPECIFIED.);
#257=B_SPLINE_CURVE_WITH_KNOTS('',3,(#11731,#11732,#11733,#11734),
 .UNSPECIFIED.,.F.,.F.,(4,4),(-4.2053902482023E-16,1.),.UNSPECIFIED.);
#258=B_SPLINE_CURVE_WITH_KNOTS('',3,(#11736,#11737,#11738,#11739),
 .UNSPECIFIED.,.F.,.F.,(4,4),(0.,1.),.UNSPECIFIED.);
#259=B_SPLINE_CURVE_WITH_KNOTS('',3,(#11741,#11742,#11743,#11744),
 .UNSPECIFIED.,.F.,.F.,(4,4),(0.,1.),.UNSPECIFIED.);
#260=B_SPLINE_CURVE_WITH_KNOTS('',3,(#11746,#11747,#11748,#11749),
 .UNSPECIFIED.,.F.,.F.,(4,4),(-4.53984320462827E-11,1.),.UNSPECIFIED.);
#261=B_SPLINE_CURVE_WITH_KNOTS('',3,(#11753,#11754,#11755,#11756),
 .UNSPECIFIED.,.F.,.F.,(4,4),(0.,0.999999968398876),.UNSPECIFIED.);
#262=B_SPLINE_CURVE_WITH_KNOTS('',3,(#11758,#11759,#11760,#11761),
 .UNSPECIFIED.,.F.,.F.,(4,4),(2.29404699546038E-7,1.),.UNSPECIFIED.);
#263=B_SPLINE_CURVE_WITH_KNOTS('',3,(#11763,#11764,#11765,#11766),
 .UNSPECIFIED.,.F.,.F.,(4,4),(0.,1.),.UNSPECIFIED.);
#264=B_SPLINE_CURVE_WITH_KNOTS('',3,(#11768,#11769,#11770,#11771),
 .UNSPECIFIED.,.F.,.F.,(4,4),(0.,1.),.UNSPECIFIED.);
#265=B_SPLINE_CURVE_WITH_KNOTS('',3,(#11773,#11774,#11775,#11776),
 .UNSPECIFIED.,.F.,.F.,(4,4),(4.99050153655672E-7,1.),.UNSPECIFIED.);
#266=B_SPLINE_CURVE_WITH_KNOTS('',3,(#11780,#11781,#11782,#11783),
 .UNSPECIFIED.,.F.,.F.,(4,4),(2.31126399320472E-7,0.999999730595559),
 .UNSPECIFIED.);
#267=B_SPLINE_CURVE_WITH_KNOTS('',3,(#11785,#11786,#11787,#11788),
 .UNSPECIFIED.,.F.,.F.,(4,4),(2.10269512148046E-16,1.),.UNSPECIFIED.);
#268=B_SPLINE_CURVE_WITH_KNOTS('',3,(#11790,#11791,#11792,#11793),
 .UNSPECIFIED.,.F.,.F.,(4,4),(0.,1.),.UNSPECIFIED.);
#269=B_SPLINE_CURVE_WITH_KNOTS('',3,(#11795,#11796,#11797,#11798),
 .UNSPECIFIED.,.F.,.F.,(4,4),(0.,1.),.UNSPECIFIED.);
#270=B_SPLINE_CURVE_WITH_KNOTS('',3,(#11800,#11801,#11802,#11803),
 .UNSPECIFIED.,.F.,.F.,(4,4),(2.35598693893978E-11,1.),.UNSPECIFIED.);
#271=B_SPLINE_CURVE_WITH_KNOTS('',3,(#11807,#11808,#11809,#11810),
 .UNSPECIFIED.,.F.,.F.,(4,4),(0.,0.999999968032225),.UNSPECIFIED.);
#272=B_SPLINE_CURVE_WITH_KNOTS('',3,(#11812,#11813,#11814,#11815),
 .UNSPECIFIED.,.F.,.F.,(4,4),(2.29317079764804E-7,1.),.UNSPECIFIED.);
#273=B_SPLINE_CURVE_WITH_KNOTS('',3,(#11817,#11818,#11819,#11820),
 .UNSPECIFIED.,.F.,.F.,(4,4),(0.,1.),.UNSPECIFIED.);
#274=B_SPLINE_CURVE_WITH_KNOTS('',3,(#11822,#11823,#11824,#11825),
 .UNSPECIFIED.,.F.,.F.,(4,4),(0.,1.),.UNSPECIFIED.);
#275=B_SPLINE_CURVE_WITH_KNOTS('',3,(#11827,#11828,#11829,#11830),
 .UNSPECIFIED.,.F.,.F.,(4,4),(4.98268763671896E-7,1.),.UNSPECIFIED.);
#276=B_SPLINE_CURVE_WITH_KNOTS('',3,(#11834,#11835,#11836,#11837),
 .UNSPECIFIED.,.F.,.F.,(4,4),(2.2953026600887E-7,0.999999729415713),
 .UNSPECIFIED.);
#277=B_SPLINE_CURVE_WITH_KNOTS('',3,(#11839,#11840,#11841,#11842),
 .UNSPECIFIED.,.F.,.F.,(4,4),(-4.20539024606654E-16,1.),.UNSPECIFIED.);
#278=B_SPLINE_CURVE_WITH_KNOTS('',3,(#11844,#11845,#11846,#11847),
 .UNSPECIFIED.,.F.,.F.,(4,4),(0.,1.),.UNSPECIFIED.);
#279=B_SPLINE_CURVE_WITH_KNOTS('',3,(#11849,#11850,#11851,#11852),
 .UNSPECIFIED.,.F.,.F.,(4,4),(0.,1.),.UNSPECIFIED.);
#280=B_SPLINE_CURVE_WITH_KNOTS('',3,(#11854,#11855,#11856,#11857),
 .UNSPECIFIED.,.F.,.F.,(4,4),(-7.09741890607156E-10,1.),.UNSPECIFIED.);
#281=B_SPLINE_CURVE_WITH_KNOTS('',3,(#11861,#11862,#11863,#11864),
 .UNSPECIFIED.,.F.,.F.,(4,4),(0.,0.999999968360085),.UNSPECIFIED.);
#282=B_SPLINE_CURVE_WITH_KNOTS('',3,(#11866,#11867,#11868,#11869),
 .UNSPECIFIED.,.F.,.F.,(4,4),(2.27631205482384E-7,1.),.UNSPECIFIED.);
#283=B_SPLINE_CURVE_WITH_KNOTS('',3,(#11871,#11872,#11873,#11874),
 .UNSPECIFIED.,.F.,.F.,(4,4),(0.,1.),.UNSPECIFIED.);
#284=B_SPLINE_CURVE_WITH_KNOTS('',3,(#11876,#11877,#11878,#11879),
 .UNSPECIFIED.,.F.,.F.,(4,4),(0.,1.),.UNSPECIFIED.);
#285=B_SPLINE_CURVE_WITH_KNOTS('',3,(#11881,#11882,#11883,#11884),
 .UNSPECIFIED.,.F.,.F.,(4,4),(4.98476028789599E-7,1.),.UNSPECIFIED.);
#286=B_SPLINE_CURVE_WITH_KNOTS('',3,(#11888,#11889,#11890,#11891),
 .UNSPECIFIED.,.F.,.F.,(4,4),(2.30300785517478E-7,0.999999730498011),
 .UNSPECIFIED.);
#287=B_SPLINE_CURVE_WITH_KNOTS('',3,(#11893,#11894,#11895,#11896),
 .UNSPECIFIED.,.F.,.F.,(4,4),(6.0851059371599E-30,1.),.UNSPECIFIED.);
#288=B_SPLINE_CURVE_WITH_KNOTS('',3,(#11898,#11899,#11900,#11901),
 .UNSPECIFIED.,.F.,.F.,(4,4),(0.,1.),.UNSPECIFIED.);
#289=B_SPLINE_CURVE_WITH_KNOTS('',3,(#11903,#11904,#11905,#11906),
 .UNSPECIFIED.,.F.,.F.,(4,4),(0.,1.),.UNSPECIFIED.);
#290=B_SPLINE_CURVE_WITH_KNOTS('',3,(#11908,#11909,#11910,#11911),
 .UNSPECIFIED.,.F.,.F.,(4,4),(-8.81759770831403E-11,1.),.UNSPECIFIED.);
#291=B_SPLINE_CURVE_WITH_KNOTS('',3,(#11915,#11916,#11917,#11918),
 .UNSPECIFIED.,.F.,.F.,(4,4),(0.,0.999999968303448),.UNSPECIFIED.);
#292=B_SPLINE_CURVE_WITH_KNOTS('',3,(#11920,#11921,#11922,#11923),
 .UNSPECIFIED.,.F.,.F.,(4,4),(2.30897813509391E-7,1.),.UNSPECIFIED.);
#293=B_SPLINE_CURVE_WITH_KNOTS('',3,(#11925,#11926,#11927,#11928),
 .UNSPECIFIED.,.F.,.F.,(4,4),(0.,1.),.UNSPECIFIED.);
#294=B_SPLINE_CURVE_WITH_KNOTS('',3,(#11930,#11931,#11932,#11933),
 .UNSPECIFIED.,.F.,.F.,(4,4),(0.,1.),.UNSPECIFIED.);
#295=B_SPLINE_CURVE_WITH_KNOTS('',3,(#11935,#11936,#11937,#11938),
 .UNSPECIFIED.,.F.,.F.,(4,4),(4.98642861198939E-7,1.),.UNSPECIFIED.);
#296=B_SPLINE_CURVE_WITH_KNOTS('',3,(#11942,#11943,#11944,#11945),
 .UNSPECIFIED.,.F.,.F.,(4,4),(2.30141277478068E-7,0.999999730101521),
 .UNSPECIFIED.);
#297=B_SPLINE_CURVE_WITH_KNOTS('',3,(#11947,#11948,#11949,#11950),
 .UNSPECIFIED.,.F.,.F.,(4,4),(0.,1.),.UNSPECIFIED.);
#298=B_SPLINE_CURVE_WITH_KNOTS('',3,(#11952,#11953,#11954,#11955),
 .UNSPECIFIED.,.F.,.F.,(4,4),(0.,1.),.UNSPECIFIED.);
#299=B_SPLINE_CURVE_WITH_KNOTS('',3,(#11957,#11958,#11959,#11960),
 .UNSPECIFIED.,.F.,.F.,(4,4),(0.,1.),.UNSPECIFIED.);
#300=B_SPLINE_CURVE_WITH_KNOTS('',3,(#11962,#11963,#11964,#11965),
 .UNSPECIFIED.,.F.,.F.,(4,4),(-3.27223686180977E-10,1.),.UNSPECIFIED.);
#301=B_SPLINE_CURVE_WITH_KNOTS('',3,(#11969,#11970,#11971,#11972),
 .UNSPECIFIED.,.F.,.F.,(4,4),(0.,0.999999968200953),.UNSPECIFIED.);
#302=B_SPLINE_CURVE_WITH_KNOTS('',3,(#11974,#11975,#11976,#11977),
 .UNSPECIFIED.,.F.,.F.,(4,4),(2.2802376939114E-7,1.),.UNSPECIFIED.);
#303=B_SPLINE_CURVE_WITH_KNOTS('',3,(#11979,#11980,#11981,#11982),
 .UNSPECIFIED.,.F.,.F.,(4,4),(0.,1.),.UNSPECIFIED.);
#304=B_SPLINE_CURVE_WITH_KNOTS('',3,(#11984,#11985,#11986,#11987),
 .UNSPECIFIED.,.F.,.F.,(4,4),(0.,1.),.UNSPECIFIED.);
#305=B_SPLINE_CURVE_WITH_KNOTS('',3,(#11989,#11990,#11991,#11992),
 .UNSPECIFIED.,.F.,.F.,(4,4),(4.98889504924982E-7,1.),.UNSPECIFIED.);
#306=B_SPLINE_CURVE_WITH_KNOTS('',3,(#11996,#11997,#11998,#11999),
 .UNSPECIFIED.,.F.,.F.,(4,4),(2.30314046378096E-7,0.99999972955559),
 .UNSPECIFIED.);
#307=B_SPLINE_CURVE_WITH_KNOTS('',3,(#12001,#12002,#12003,#12004),
 .UNSPECIFIED.,.F.,.F.,(4,4),(-4.2053902482023E-16,1.),.UNSPECIFIED.);
#308=B_SPLINE_CURVE_WITH_KNOTS('',3,(#12006,#12007,#12008,#12009),
 .UNSPECIFIED.,.F.,.F.,(4,4),(0.,1.),.UNSPECIFIED.);
#309=B_SPLINE_CURVE_WITH_KNOTS('',3,(#12011,#12012,#12013,#12014),
 .UNSPECIFIED.,.F.,.F.,(4,4),(0.,1.),.UNSPECIFIED.);
#310=B_SPLINE_CURVE_WITH_KNOTS('',3,(#12016,#12017,#12018,#12019),
 .UNSPECIFIED.,.F.,.F.,(4,4),(-4.06438355921804E-10,1.),.UNSPECIFIED.);
#311=B_SPLINE_CURVE_WITH_KNOTS('',3,(#12023,#12024,#12025,#12026),
 .UNSPECIFIED.,.F.,.F.,(4,4),(0.,0.999999968218356),.UNSPECIFIED.);
#312=B_SPLINE_CURVE_WITH_KNOTS('',3,(#12028,#12029,#12030,#12031),
 .UNSPECIFIED.,.F.,.F.,(4,4),(2.29788204199464E-7,1.),.UNSPECIFIED.);
#313=B_SPLINE_CURVE_WITH_KNOTS('',3,(#12033,#12034,#12035,#12036),
 .UNSPECIFIED.,.F.,.F.,(4,4),(0.,1.),.UNSPECIFIED.);
#314=B_SPLINE_CURVE_WITH_KNOTS('',3,(#12038,#12039,#12040,#12041),
 .UNSPECIFIED.,.F.,.F.,(4,4),(0.,1.),.UNSPECIFIED.);
#315=B_SPLINE_CURVE_WITH_KNOTS('',3,(#12043,#12044,#12045,#12046),
 .UNSPECIFIED.,.F.,.F.,(4,4),(4.99050153655672E-7,1.),.UNSPECIFIED.);
#316=B_SPLINE_CURVE_WITH_KNOTS('',3,(#12050,#12051,#12052,#12053),
 .UNSPECIFIED.,.F.,.F.,(4,4),(2.3112639881784E-7,0.999999730979069),
 .UNSPECIFIED.);
#317=B_SPLINE_CURVE_WITH_KNOTS('',3,(#12055,#12056,#12057,#12058),
 .UNSPECIFIED.,.F.,.F.,(4,4),(2.10269512148046E-16,1.),.UNSPECIFIED.);
#318=B_SPLINE_CURVE_WITH_KNOTS('',3,(#12060,#12061,#12062,#12063),
 .UNSPECIFIED.,.F.,.F.,(4,4),(0.,1.),.UNSPECIFIED.);
#319=B_SPLINE_CURVE_WITH_KNOTS('',3,(#12065,#12066,#12067,#12068),
 .UNSPECIFIED.,.F.,.F.,(4,4),(0.,1.),.UNSPECIFIED.);
#320=B_SPLINE_CURVE_WITH_KNOTS('',3,(#12070,#12071,#12072,#12073),
 .UNSPECIFIED.,.F.,.F.,(4,4),(2.49280919609535E-10,1.),.UNSPECIFIED.);
#321=B_SPLINE_CURVE_WITH_KNOTS('',3,(#12077,#12078,#12079,#12080),
 .UNSPECIFIED.,.F.,.F.,(4,4),(0.,0.999999968145085),.UNSPECIFIED.);
#322=B_SPLINE_CURVE_WITH_KNOTS('',3,(#12082,#12083,#12084,#12085),
 .UNSPECIFIED.,.F.,.F.,(4,4),(2.29700583941174E-7,1.),.UNSPECIFIED.);
#323=B_SPLINE_CURVE_WITH_KNOTS('',3,(#12087,#12088,#12089,#12090),
 .UNSPECIFIED.,.F.,.F.,(4,4),(0.,1.),.UNSPECIFIED.);
#324=B_SPLINE_CURVE_WITH_KNOTS('',3,(#12092,#12093,#12094,#12095),
 .UNSPECIFIED.,.F.,.F.,(4,4),(0.,1.),.UNSPECIFIED.);
#325=B_SPLINE_CURVE_WITH_KNOTS('',3,(#12097,#12098,#12099,#12100),
 .UNSPECIFIED.,.F.,.F.,(4,4),(4.98268763671896E-7,1.),.UNSPECIFIED.);
#326=B_SPLINE_CURVE_WITH_KNOTS('',3,(#12104,#12105,#12106,#12107),
 .UNSPECIFIED.,.F.,.F.,(4,4),(2.29530277201637E-7,0.999999729799226),
 .UNSPECIFIED.);
#327=B_SPLINE_CURVE_WITH_KNOTS('',3,(#12109,#12110,#12111,#12112),
 .UNSPECIFIED.,.F.,.F.,(4,4),(-4.20539024606654E-16,1.),.UNSPECIFIED.);
#328=B_SPLINE_CURVE_WITH_KNOTS('',3,(#12114,#12115,#12116,#12117),
 .UNSPECIFIED.,.F.,.F.,(4,4),(0.,1.),.UNSPECIFIED.);
#329=B_SPLINE_CURVE_WITH_KNOTS('',3,(#12119,#12120,#12121,#12122),
 .UNSPECIFIED.,.F.,.F.,(4,4),(0.,1.),.UNSPECIFIED.);
#330=B_SPLINE_CURVE_WITH_KNOTS('',3,(#12124,#12125,#12126,#12127),
 .UNSPECIFIED.,.F.,.F.,(4,4),(-4.84020982613384E-10,1.),.UNSPECIFIED.);
#331=B_SPLINE_CURVE_WITH_KNOTS('',3,(#12131,#12132,#12133,#12134),
 .UNSPECIFIED.,.F.,.F.,(4,4),(0.,0.999999968179565),.UNSPECIFIED.);
#332=B_SPLINE_CURVE_WITH_KNOTS('',3,(#12136,#12137,#12138,#12139),
 .UNSPECIFIED.,.F.,.F.,(4,4),(2.27017792871544E-7,1.),.UNSPECIFIED.);
#333=B_SPLINE_CURVE_WITH_KNOTS('',3,(#12141,#12142,#12143,#12144),
 .UNSPECIFIED.,.F.,.F.,(4,4),(0.,1.),.UNSPECIFIED.);
#334=B_SPLINE_CURVE_WITH_KNOTS('',3,(#12146,#12147,#12148,#12149),
 .UNSPECIFIED.,.F.,.F.,(4,4),(0.,1.),.UNSPECIFIED.);
#335=B_SPLINE_CURVE_WITH_KNOTS('',3,(#12151,#12152,#12153,#12154),
 .UNSPECIFIED.,.F.,.F.,(4,4),(4.98476028789599E-7,1.),.UNSPECIFIED.);
#336=B_SPLINE_CURVE_WITH_KNOTS('',3,(#12158,#12159,#12160,#12161),
 .UNSPECIFIED.,.F.,.F.,(4,4),(2.30300766849461E-7,0.999999729884583),
 .UNSPECIFIED.);
#337=B_SPLINE_CURVE_WITH_KNOTS('',3,(#12163,#12164,#12165,#12166),
 .UNSPECIFIED.,.F.,.F.,(4,4),(6.0851059371599E-30,1.),.UNSPECIFIED.);
#338=B_SPLINE_CURVE_WITH_KNOTS('',3,(#12168,#12169,#12170,#12171),
 .UNSPECIFIED.,.F.,.F.,(4,4),(0.,1.),.UNSPECIFIED.);
#339=B_SPLINE_CURVE_WITH_KNOTS('',3,(#12173,#12174,#12175,#12176),
 .UNSPECIFIED.,.F.,.F.,(4,4),(0.,1.),.UNSPECIFIED.);
#340=B_SPLINE_CURVE_WITH_KNOTS('',3,(#12178,#12179,#12180,#12181),
 .UNSPECIFIED.,.F.,.F.,(4,4),(-4.49216403355802E-10,1.),.UNSPECIFIED.);
#341=B_SPLINE_CURVE_WITH_KNOTS('',3,(#12185,#12186,#12187,#12188),
 .UNSPECIFIED.,.F.,.F.,(4,4),(0.,0.999999968416308),.UNSPECIFIED.);
#342=B_SPLINE_CURVE_WITH_KNOTS('',3,(#12190,#12191,#12192,#12193),
 .UNSPECIFIED.,.F.,.F.,(4,4),(2.31281316829358E-7,1.),.UNSPECIFIED.);
#343=B_SPLINE_CURVE_WITH_KNOTS('',3,(#12195,#12196,#12197,#12198),
 .UNSPECIFIED.,.F.,.F.,(4,4),(0.,1.),.UNSPECIFIED.);
#344=B_SPLINE_CURVE_WITH_KNOTS('',3,(#12200,#12201,#12202,#12203),
 .UNSPECIFIED.,.F.,.F.,(4,4),(0.,1.),.UNSPECIFIED.);
#345=B_SPLINE_CURVE_WITH_KNOTS('',3,(#12205,#12206,#12207,#12208),
 .UNSPECIFIED.,.F.,.F.,(4,4),(4.98642861198939E-7,1.),.UNSPECIFIED.);
#346=B_SPLINE_CURVE_WITH_KNOTS('',3,(#12212,#12213,#12214,#12215),
 .UNSPECIFIED.,.F.,.F.,(4,4),(2.30141291313089E-7,0.99999973030602),
 .UNSPECIFIED.);
#347=B_SPLINE_CURVE_WITH_KNOTS('',3,(#12217,#12218,#12219,#12220),
 .UNSPECIFIED.,.F.,.F.,(4,4),(0.,1.),.UNSPECIFIED.);
#348=B_SPLINE_CURVE_WITH_KNOTS('',3,(#12222,#12223,#12224,#12225),
 .UNSPECIFIED.,.F.,.F.,(4,4),(0.,1.),.UNSPECIFIED.);
#349=B_SPLINE_CURVE_WITH_KNOTS('',3,(#12227,#12228,#12229,#12230),
 .UNSPECIFIED.,.F.,.F.,(4,4),(0.,1.),.UNSPECIFIED.);
#350=B_SPLINE_CURVE_WITH_KNOTS('',3,(#12232,#12233,#12234,#12235),
 .UNSPECIFIED.,.F.,.F.,(4,4),(-1.72817946408447E-10,1.),.UNSPECIFIED.);
#351=B_SPLINE_CURVE_WITH_KNOTS('',3,(#12239,#12240,#12241,#12242),
 .UNSPECIFIED.,.F.,.F.,(4,4),(0.,0.999999968261127),.UNSPECIFIED.);
#352=B_SPLINE_CURVE_WITH_KNOTS('',3,(#12244,#12245,#12246,#12247),
 .UNSPECIFIED.,.F.,.F.,(4,4),(2.28228239255696E-7,1.),.UNSPECIFIED.);
#353=B_SPLINE_CURVE_WITH_KNOTS('',3,(#12249,#12250,#12251,#12252),
 .UNSPECIFIED.,.F.,.F.,(4,4),(0.,1.),.UNSPECIFIED.);
#354=B_SPLINE_CURVE_WITH_KNOTS('',3,(#12254,#12255,#12256,#12257),
 .UNSPECIFIED.,.F.,.F.,(4,4),(0.,1.),.UNSPECIFIED.);
#355=B_SPLINE_CURVE_WITH_KNOTS('',3,(#12259,#12260,#12261,#12262),
 .UNSPECIFIED.,.F.,.F.,(4,4),(4.98889504924982E-7,1.),.UNSPECIFIED.);
#356=B_SPLINE_CURVE_WITH_KNOTS('',3,(#12266,#12267,#12268,#12269),
 .UNSPECIFIED.,.F.,.F.,(4,4),(2.30314020679759E-7,0.999999729760012),
 .UNSPECIFIED.);
#357=B_SPLINE_CURVE_WITH_KNOTS('',3,(#12271,#12272,#12273,#12274),
 .UNSPECIFIED.,.F.,.F.,(4,4),(-4.2053902482023E-16,1.),.UNSPECIFIED.);
#358=B_SPLINE_CURVE_WITH_KNOTS('',3,(#12276,#12277,#12278,#12279),
 .UNSPECIFIED.,.F.,.F.,(4,4),(0.,1.),.UNSPECIFIED.);
#359=B_SPLINE_CURVE_WITH_KNOTS('',3,(#12281,#12282,#12283,#12284),
 .UNSPECIFIED.,.F.,.F.,(4,4),(0.,1.),.UNSPECIFIED.);
#360=B_SPLINE_CURVE_WITH_KNOTS('',3,(#12286,#12287,#12288,#12289),
 .UNSPECIFIED.,.F.,.F.,(4,4),(-2.86092757243134E-10,1.),.UNSPECIFIED.);
#361=B_SPLINE_CURVE_WITH_KNOTS('',3,(#12293,#12294,#12295,#12296),
 .UNSPECIFIED.,.F.,.F.,(4,4),(0.,0.999999968278529),.UNSPECIFIED.);
#362=B_SPLINE_CURVE_WITH_KNOTS('',3,(#12298,#12299,#12300,#12301),
 .UNSPECIFIED.,.F.,.F.,(4,4),(2.28995756837677E-7,1.),.UNSPECIFIED.);
#363=B_SPLINE_CURVE_WITH_KNOTS('',3,(#12303,#12304,#12305,#12306),
 .UNSPECIFIED.,.F.,.F.,(4,4),(0.,1.),.UNSPECIFIED.);
#364=B_SPLINE_CURVE_WITH_KNOTS('',3,(#12308,#12309,#12310,#12311),
 .UNSPECIFIED.,.F.,.F.,(4,4),(0.,1.),.UNSPECIFIED.);
#365=B_SPLINE_CURVE_WITH_KNOTS('',3,(#12313,#12314,#12315,#12316),
 .UNSPECIFIED.,.F.,.F.,(4,4),(4.99050153655672E-7,1.),.UNSPECIFIED.);
#366=B_SPLINE_CURVE_WITH_KNOTS('',3,(#12320,#12321,#12322,#12323),
 .UNSPECIFIED.,.F.,.F.,(4,4),(2.31126418142628E-7,0.999999730186638),
 .UNSPECIFIED.);
#367=B_SPLINE_CURVE_WITH_KNOTS('',3,(#12325,#12326,#12327,#12328),
 .UNSPECIFIED.,.F.,.F.,(4,4),(2.10269512148046E-16,1.),.UNSPECIFIED.);
#368=B_SPLINE_CURVE_WITH_KNOTS('',3,(#12330,#12331,#12332,#12333),
 .UNSPECIFIED.,.F.,.F.,(4,4),(0.,1.),.UNSPECIFIED.);
#369=B_SPLINE_CURVE_WITH_KNOTS('',3,(#12335,#12336,#12337,#12338),
 .UNSPECIFIED.,.F.,.F.,(4,4),(0.,1.),.UNSPECIFIED.);
#370=B_SPLINE_CURVE_WITH_KNOTS('',3,(#12340,#12341,#12342,#12343),
 .UNSPECIFIED.,.F.,.F.,(4,4),(-2.17133087511602E-10,1.),.UNSPECIFIED.);
#371=B_SPLINE_CURVE_WITH_KNOTS('',3,(#12347,#12348,#12349,#12350),
 .UNSPECIFIED.,.F.,.F.,(4,4),(0.,0.999999968205259),.UNSPECIFIED.);
#372=B_SPLINE_CURVE_WITH_KNOTS('',3,(#12352,#12353,#12354,#12355),
 .UNSPECIFIED.,.F.,.F.,(4,4),(2.29905056582326E-7,1.),.UNSPECIFIED.);
#373=B_SPLINE_CURVE_WITH_KNOTS('',3,(#12357,#12358,#12359,#12360),
 .UNSPECIFIED.,.F.,.F.,(4,4),(0.,1.),.UNSPECIFIED.);
#374=B_SPLINE_CURVE_WITH_KNOTS('',3,(#12362,#12363,#12364,#12365),
 .UNSPECIFIED.,.F.,.F.,(4,4),(0.,1.),.UNSPECIFIED.);
#375=B_SPLINE_CURVE_WITH_KNOTS('',3,(#12367,#12368,#12369,#12370),
 .UNSPECIFIED.,.F.,.F.,(4,4),(4.98268763671896E-7,1.),.UNSPECIFIED.);
#376=B_SPLINE_CURVE_WITH_KNOTS('',3,(#12374,#12375,#12376,#12377),
 .UNSPECIFIED.,.F.,.F.,(4,4),(2.29530257876848E-7,0.99999973000367),
 .UNSPECIFIED.);
#377=B_SPLINE_CURVE_WITH_KNOTS('',3,(#12379,#12380,#12381,#12382),
 .UNSPECIFIED.,.F.,.F.,(4,4),(-4.20539024606654E-16,1.),.UNSPECIFIED.);
#378=B_SPLINE_CURVE_WITH_KNOTS('',3,(#12384,#12385,#12386,#12387),
 .UNSPECIFIED.,.F.,.F.,(4,4),(0.,1.),.UNSPECIFIED.);
#379=B_SPLINE_CURVE_WITH_KNOTS('',3,(#12389,#12390,#12391,#12392),
 .UNSPECIFIED.,.F.,.F.,(4,4),(0.,1.),.UNSPECIFIED.);
#380=B_SPLINE_CURVE_WITH_KNOTS('',3,(#12394,#12395,#12396,#12397),
 .UNSPECIFIED.,.F.,.F.,(4,4),(-3.63673936213342E-10,1.),.UNSPECIFIED.);
#381=B_SPLINE_CURVE_WITH_KNOTS('',3,(#12401,#12402,#12403,#12404),
 .UNSPECIFIED.,.F.,.F.,(4,4),(0.,0.999999968239738),.UNSPECIFIED.);
#382=B_SPLINE_CURVE_WITH_KNOTS('',3,(#12406,#12407,#12408,#12409),
 .UNSPECIFIED.,.F.,.F.,(4,4),(2.27222261671625E-7,1.),.UNSPECIFIED.);
#383=B_SPLINE_CURVE_WITH_KNOTS('',3,(#12411,#12412,#12413,#12414),
 .UNSPECIFIED.,.F.,.F.,(4,4),(0.,1.),.UNSPECIFIED.);
#384=B_SPLINE_CURVE_WITH_KNOTS('',3,(#12416,#12417,#12418,#12419),
 .UNSPECIFIED.,.F.,.F.,(4,4),(0.,1.),.UNSPECIFIED.);
#385=B_SPLINE_CURVE_WITH_KNOTS('',3,(#12421,#12422,#12423,#12424),
 .UNSPECIFIED.,.F.,.F.,(4,4),(4.98476028789599E-7,1.),.UNSPECIFIED.);
#386=B_SPLINE_CURVE_WITH_KNOTS('',3,(#12428,#12429,#12430,#12431),
 .UNSPECIFIED.,.F.,.F.,(4,4),(2.30300789875764E-7,0.999999730089088),
 .UNSPECIFIED.);
#387=B_SPLINE_CURVE_WITH_KNOTS('',3,(#12433,#12434,#12435,#12436),
 .UNSPECIFIED.,.F.,.F.,(4,4),(6.0851059371599E-30,1.),.UNSPECIFIED.);
#388=B_SPLINE_CURVE_WITH_KNOTS('',3,(#12438,#12439,#12440,#12441),
 .UNSPECIFIED.,.F.,.F.,(4,4),(0.,1.),.UNSPECIFIED.);
#389=B_SPLINE_CURVE_WITH_KNOTS('',3,(#12443,#12444,#12445,#12446),
 .UNSPECIFIED.,.F.,.F.,(4,4),(0.,1.),.UNSPECIFIED.);
#390=B_SPLINE_CURVE_WITH_KNOTS('',3,(#12448,#12449,#12450,#12451),
 .UNSPECIFIED.,.F.,.F.,(4,4),(-3.28868497233371E-10,1.),.UNSPECIFIED.);
#391=B_SPLINE_CURVE_WITH_KNOTS('',3,(#12455,#12456,#12457,#12458),
 .UNSPECIFIED.,.F.,.F.,(4,4),(0.,0.999999968183101),.UNSPECIFIED.);
#392=B_SPLINE_CURVE_WITH_KNOTS('',3,(#12460,#12461,#12462,#12463),
 .UNSPECIFIED.,.F.,.F.,(4,4),(2.30488871044787E-7,1.),.UNSPECIFIED.);
#393=B_SPLINE_CURVE_WITH_KNOTS('',3,(#12465,#12466,#12467,#12468),
 .UNSPECIFIED.,.F.,.F.,(4,4),(0.,1.),.UNSPECIFIED.);
#394=B_SPLINE_CURVE_WITH_KNOTS('',3,(#12470,#12471,#12472,#12473),
 .UNSPECIFIED.,.F.,.F.,(4,4),(0.,0.999999996212121),.UNSPECIFIED.);
#395=B_SPLINE_CURVE_WITH_KNOTS('',3,(#12480,#12481,#12482,#12483),
 .UNSPECIFIED.,.F.,.F.,(4,4),(1.24500014464512E-7,0.999999750000014),
 .UNSPECIFIED.);
#396=B_SPLINE_CURVE_WITH_KNOTS('',3,(#12485,#12486,#12487,#12488),
 .UNSPECIFIED.,.F.,.F.,(4,4),(1.6055290347619E-11,1.),.UNSPECIFIED.);
#397=B_SPLINE_CURVE_WITH_KNOTS('',3,(#12490,#12491,#12492,#12493),
 .UNSPECIFIED.,.F.,.F.,(4,4),(-1.38777878078144E-14,0.999999999999986),
 .UNSPECIFIED.);
#398=B_SPLINE_CURVE_WITH_KNOTS('',3,(#12495,#12496,#12497,#12498),
 .UNSPECIFIED.,.F.,.F.,(4,4),(0.,0.999999945331273),.UNSPECIFIED.);
#399=B_SPLINE_CURVE_WITH_KNOTS('',3,(#12500,#12501,#12502,#12503),
 .UNSPECIFIED.,.F.,.F.,(4,4),(1.24500014464512E-7,0.999999750000014),
 .UNSPECIFIED.);
#400=B_SPLINE_CURVE_WITH_KNOTS('',3,(#12507,#12508,#12509,#12510),
 .UNSPECIFIED.,.F.,.F.,(4,4),(0.,1.),.UNSPECIFIED.);
#401=B_SPLINE_CURVE_WITH_KNOTS('',3,(#12511,#12512,#12513,#12514),
 .UNSPECIFIED.,.F.,.F.,(4,4),(0.,1.),.UNSPECIFIED.);
#402=B_SPLINE_CURVE_WITH_KNOTS('',3,(#12518,#12519,#12520,#12521),
 .UNSPECIFIED.,.F.,.F.,(4,4),(0.,1.),.UNSPECIFIED.);
#403=B_SPLINE_CURVE_WITH_KNOTS('',3,(#12522,#12523,#12524,#12525),
 .UNSPECIFIED.,.F.,.F.,(4,4),(0.,1.),.UNSPECIFIED.);
#404=B_SPLINE_CURVE_WITH_KNOTS('',3,(#12529,#12530,#12531,#12532),
 .UNSPECIFIED.,.F.,.F.,(4,4),(0.,1.),.UNSPECIFIED.);
#405=B_SPLINE_CURVE_WITH_KNOTS('',3,(#12533,#12534,#12535,#12536),
 .UNSPECIFIED.,.F.,.F.,(4,4),(0.,1.),.UNSPECIFIED.);
#406=B_SPLINE_CURVE_WITH_KNOTS('',3,(#12540,#12541,#12542,#12543),
 .UNSPECIFIED.,.F.,.F.,(4,4),(0.,1.),.UNSPECIFIED.);
#407=B_SPLINE_CURVE_WITH_KNOTS('',3,(#12544,#12545,#12546,#12547),
 .UNSPECIFIED.,.F.,.F.,(4,4),(0.,1.),.UNSPECIFIED.);
#408=B_SPLINE_CURVE_WITH_KNOTS('',3,(#12551,#12552,#12553,#12554),
 .UNSPECIFIED.,.F.,.F.,(4,4),(0.,1.),.UNSPECIFIED.);
#409=B_SPLINE_CURVE_WITH_KNOTS('',3,(#12555,#12556,#12557,#12558),
 .UNSPECIFIED.,.F.,.F.,(4,4),(0.,1.),.UNSPECIFIED.);
#410=B_SPLINE_CURVE_WITH_KNOTS('',3,(#12562,#12563,#12564,#12565),
 .UNSPECIFIED.,.F.,.F.,(4,4),(0.,1.),.UNSPECIFIED.);
#411=B_SPLINE_CURVE_WITH_KNOTS('',3,(#12566,#12567,#12568,#12569),
 .UNSPECIFIED.,.F.,.F.,(4,4),(0.,1.),.UNSPECIFIED.);
#412=B_SPLINE_CURVE_WITH_KNOTS('',3,(#12573,#12574,#12575,#12576),
 .UNSPECIFIED.,.F.,.F.,(4,4),(0.,1.),.UNSPECIFIED.);
#413=B_SPLINE_CURVE_WITH_KNOTS('',3,(#12577,#12578,#12579,#12580),
 .UNSPECIFIED.,.F.,.F.,(4,4),(0.,1.),.UNSPECIFIED.);
#414=B_SPLINE_CURVE_WITH_KNOTS('',3,(#12584,#12585,#12586,#12587),
 .UNSPECIFIED.,.F.,.F.,(4,4),(0.,1.),.UNSPECIFIED.);
#415=B_SPLINE_CURVE_WITH_KNOTS('',3,(#12588,#12589,#12590,#12591),
 .UNSPECIFIED.,.F.,.F.,(4,4),(0.,1.),.UNSPECIFIED.);
#416=B_SPLINE_CURVE_WITH_KNOTS('',3,(#12595,#12596,#12597,#12598),
 .UNSPECIFIED.,.F.,.F.,(4,4),(0.,1.),.UNSPECIFIED.);
#417=B_SPLINE_CURVE_WITH_KNOTS('',3,(#12599,#12600,#12601,#12602),
 .UNSPECIFIED.,.F.,.F.,(4,4),(0.,1.),.UNSPECIFIED.);
#418=B_SPLINE_CURVE_WITH_KNOTS('',3,(#12607,#12608,#12609,#12610),
 .UNSPECIFIED.,.F.,.F.,(4,4),(0.,1.),.UNSPECIFIED.);
#419=B_SPLINE_CURVE_WITH_KNOTS('',3,(#12611,#12612,#12613,#12614),
 .UNSPECIFIED.,.F.,.F.,(4,4),(0.,1.),.UNSPECIFIED.);
#420=B_SPLINE_CURVE_WITH_KNOTS('',3,(#12618,#12619,#12620,#12621),
 .UNSPECIFIED.,.F.,.F.,(4,4),(0.,1.),.UNSPECIFIED.);
#421=B_SPLINE_CURVE_WITH_KNOTS('',3,(#12622,#12623,#12624,#12625),
 .UNSPECIFIED.,.F.,.F.,(4,4),(0.,1.),.UNSPECIFIED.);
#422=B_SPLINE_CURVE_WITH_KNOTS('',3,(#12629,#12630,#12631,#12632),
 .UNSPECIFIED.,.F.,.F.,(4,4),(0.,1.),.UNSPECIFIED.);
#423=B_SPLINE_CURVE_WITH_KNOTS('',3,(#12633,#12634,#12635,#12636),
 .UNSPECIFIED.,.F.,.F.,(4,4),(0.,1.),.UNSPECIFIED.);
#424=B_SPLINE_CURVE_WITH_KNOTS('',3,(#12640,#12641,#12642,#12643),
 .UNSPECIFIED.,.F.,.F.,(4,4),(0.,1.),.UNSPECIFIED.);
#425=B_SPLINE_CURVE_WITH_KNOTS('',3,(#12644,#12645,#12646,#12647),
 .UNSPECIFIED.,.F.,.F.,(4,4),(0.,1.),.UNSPECIFIED.);
#426=B_SPLINE_CURVE_WITH_KNOTS('',3,(#12651,#12652,#12653,#12654),
 .UNSPECIFIED.,.F.,.F.,(4,4),(0.,1.),.UNSPECIFIED.);
#427=B_SPLINE_CURVE_WITH_KNOTS('',3,(#12655,#12656,#12657,#12658),
 .UNSPECIFIED.,.F.,.F.,(4,4),(0.,1.),.UNSPECIFIED.);
#428=B_SPLINE_CURVE_WITH_KNOTS('',3,(#12662,#12663,#12664,#12665),
 .UNSPECIFIED.,.F.,.F.,(4,4),(0.,1.),.UNSPECIFIED.);
#429=B_SPLINE_CURVE_WITH_KNOTS('',3,(#12666,#12667,#12668,#12669),
 .UNSPECIFIED.,.F.,.F.,(4,4),(0.,1.),.UNSPECIFIED.);
#430=B_SPLINE_CURVE_WITH_KNOTS('',3,(#12673,#12674,#12675,#12676),
 .UNSPECIFIED.,.F.,.F.,(4,4),(0.,1.),.UNSPECIFIED.);
#431=B_SPLINE_CURVE_WITH_KNOTS('',3,(#12677,#12678,#12679,#12680),
 .UNSPECIFIED.,.F.,.F.,(4,4),(0.,1.),.UNSPECIFIED.);
#432=B_SPLINE_CURVE_WITH_KNOTS('',3,(#12684,#12685,#12686,#12687),
 .UNSPECIFIED.,.F.,.F.,(4,4),(0.,1.),.UNSPECIFIED.);
#433=B_SPLINE_CURVE_WITH_KNOTS('',3,(#12688,#12689,#12690,#12691),
 .UNSPECIFIED.,.F.,.F.,(4,4),(0.,1.),.UNSPECIFIED.);
#434=B_SPLINE_CURVE_WITH_KNOTS('',3,(#12695,#12696,#12697,#12698),
 .UNSPECIFIED.,.F.,.F.,(4,4),(0.,1.),.UNSPECIFIED.);
#435=B_SPLINE_CURVE_WITH_KNOTS('',3,(#12699,#12700,#12701,#12702),
 .UNSPECIFIED.,.F.,.F.,(4,4),(0.,1.),.UNSPECIFIED.);
#436=B_SPLINE_CURVE_WITH_KNOTS('',3,(#12706,#12707,#12708,#12709),
 .UNSPECIFIED.,.F.,.F.,(4,4),(0.,1.),.UNSPECIFIED.);
#437=B_SPLINE_CURVE_WITH_KNOTS('',3,(#12715,#12716,#12717,#12718),
 .UNSPECIFIED.,.F.,.F.,(4,4),(0.,1.),.UNSPECIFIED.);
#438=B_SPLINE_CURVE_WITH_KNOTS('',3,(#12720,#12721,#12722,#12723),
 .UNSPECIFIED.,.F.,.F.,(4,4),(0.,1.),.UNSPECIFIED.);
#439=B_SPLINE_CURVE_WITH_KNOTS('',3,(#12727,#12728,#12729,#12730),
 .UNSPECIFIED.,.F.,.F.,(4,4),(0.,1.),.UNSPECIFIED.);
#440=B_SPLINE_CURVE_WITH_KNOTS('',3,(#12732,#12733,#12734,#12735),
 .UNSPECIFIED.,.F.,.F.,(4,4),(0.,0.999999999884541),.UNSPECIFIED.);
#441=B_SPLINE_CURVE_WITH_KNOTS('',3,(#12739,#12740,#12741,#12742),
 .UNSPECIFIED.,.F.,.F.,(4,4),(0.,1.),.UNSPECIFIED.);
#442=B_SPLINE_CURVE_WITH_KNOTS('',3,(#12744,#12745,#12746,#12747),
 .UNSPECIFIED.,.F.,.F.,(4,4),(0.,1.),.UNSPECIFIED.);
#443=B_SPLINE_CURVE_WITH_KNOTS('',3,(#12751,#12752,#12753,#12754),
 .UNSPECIFIED.,.F.,.F.,(4,4),(0.,1.),.UNSPECIFIED.);
#444=B_SPLINE_CURVE_WITH_KNOTS('',3,(#12756,#12757,#12758,#12759),
 .UNSPECIFIED.,.F.,.F.,(4,4),(0.,0.999999999942397),.UNSPECIFIED.);
#445=B_SPLINE_CURVE_WITH_KNOTS('',3,(#12763,#12764,#12765,#12766),
 .UNSPECIFIED.,.F.,.F.,(4,4),(0.,1.),.UNSPECIFIED.);
#446=B_SPLINE_CURVE_WITH_KNOTS('',3,(#12768,#12769,#12770,#12771),
 .UNSPECIFIED.,.F.,.F.,(4,4),(0.,0.999999999818942),.UNSPECIFIED.);
#447=B_SPLINE_CURVE_WITH_KNOTS('',3,(#12775,#12776,#12777,#12778),
 .UNSPECIFIED.,.F.,.F.,(4,4),(0.,1.),.UNSPECIFIED.);
#448=B_SPLINE_CURVE_WITH_KNOTS('',3,(#12780,#12781,#12782,#12783),
 .UNSPECIFIED.,.F.,.F.,(4,4),(0.,1.),.UNSPECIFIED.);
#449=B_SPLINE_CURVE_WITH_KNOTS('',3,(#12787,#12788,#12789,#12790),
 .UNSPECIFIED.,.F.,.F.,(4,4),(0.,1.),.UNSPECIFIED.);
#450=B_SPLINE_CURVE_WITH_KNOTS('',3,(#12792,#12793,#12794,#12795),
 .UNSPECIFIED.,.F.,.F.,(4,4),(0.,0.999999999944715),.UNSPECIFIED.);
#451=B_SPLINE_CURVE_WITH_KNOTS('',3,(#12799,#12800,#12801,#12802),
 .UNSPECIFIED.,.F.,.F.,(4,4),(0.,1.),.UNSPECIFIED.);
#452=B_SPLINE_CURVE_WITH_KNOTS('',3,(#12804,#12805,#12806,#12807),
 .UNSPECIFIED.,.F.,.F.,(4,4),(0.,1.),.UNSPECIFIED.);
#453=B_SPLINE_CURVE_WITH_KNOTS('',3,(#12811,#12812,#12813,#12814),
 .UNSPECIFIED.,.F.,.F.,(4,4),(0.,1.),.UNSPECIFIED.);
#454=B_SPLINE_CURVE_WITH_KNOTS('',3,(#12816,#12817,#12818,#12819),
 .UNSPECIFIED.,.F.,.F.,(4,4),(0.,1.00000000000257),.UNSPECIFIED.);
#455=B_SPLINE_CURVE_WITH_KNOTS('',3,(#12823,#12824,#12825,#12826),
 .UNSPECIFIED.,.F.,.F.,(4,4),(1.6055290347619E-11,1.),.UNSPECIFIED.);
#456=B_SPLINE_CURVE_WITH_KNOTS('',3,(#12828,#12829,#12830,#12831),
 .UNSPECIFIED.,.F.,.F.,(4,4),(0.,0.999999999931802),.UNSPECIFIED.);
#457=B_SPLINE_CURVE_WITH_KNOTS('',3,(#12835,#12836,#12837,#12838),
 .UNSPECIFIED.,.F.,.F.,(4,4),(0.,1.),.UNSPECIFIED.);
#458=B_SPLINE_CURVE_WITH_KNOTS('',3,(#12840,#12841,#12842,#12843),
 .UNSPECIFIED.,.F.,.F.,(4,4),(0.,0.999999999920396),.UNSPECIFIED.);
#459=B_SPLINE_CURVE_WITH_KNOTS('',3,(#12847,#12848,#12849,#12850),
 .UNSPECIFIED.,.F.,.F.,(4,4),(0.,1.),.UNSPECIFIED.);
#460=B_SPLINE_CURVE_WITH_KNOTS('',3,(#12852,#12853,#12854,#12855),
 .UNSPECIFIED.,.F.,.F.,(4,4),(0.,1.),.UNSPECIFIED.);
#461=B_SPLINE_CURVE_WITH_KNOTS('',3,(#12859,#12860,#12861,#12862),
 .UNSPECIFIED.,.F.,.F.,(4,4),(0.,1.),.UNSPECIFIED.);
#462=B_SPLINE_CURVE_WITH_KNOTS('',3,(#12864,#12865,#12866,#12867),
 .UNSPECIFIED.,.F.,.F.,(4,4),(0.,0.999999999923948),.UNSPECIFIED.);
#463=B_SPLINE_CURVE_WITH_KNOTS('',3,(#12871,#12872,#12873,#12874),
 .UNSPECIFIED.,.F.,.F.,(4,4),(0.,1.),.UNSPECIFIED.);
#464=B_SPLINE_CURVE_WITH_KNOTS('',3,(#12876,#12877,#12878,#12879),
 .UNSPECIFIED.,.F.,.F.,(4,4),(0.,1.),.UNSPECIFIED.);
#465=B_SPLINE_CURVE_WITH_KNOTS('',3,(#12883,#12884,#12885,#12886),
 .UNSPECIFIED.,.F.,.F.,(4,4),(0.,1.),.UNSPECIFIED.);
#466=B_SPLINE_CURVE_WITH_KNOTS('',3,(#12888,#12889,#12890,#12891),
 .UNSPECIFIED.,.F.,.F.,(4,4),(0.,0.999999999991978),.UNSPECIFIED.);
#467=B_SPLINE_CURVE_WITH_KNOTS('',3,(#12895,#12896,#12897,#12898),
 .UNSPECIFIED.,.F.,.F.,(4,4),(0.,1.),.UNSPECIFIED.);
#468=B_SPLINE_CURVE_WITH_KNOTS('',3,(#12900,#12901,#12902,#12903),
 .UNSPECIFIED.,.F.,.F.,(4,4),(0.,0.999999999980569),.UNSPECIFIED.);
#469=B_SPLINE_CURVE_WITH_KNOTS('',3,(#12907,#12908,#12909,#12910),
 .UNSPECIFIED.,.F.,.F.,(4,4),(0.,1.),.UNSPECIFIED.);
#470=B_SPLINE_CURVE_WITH_KNOTS('',3,(#12912,#12913,#12914,#12915),
 .UNSPECIFIED.,.F.,.F.,(4,4),(0.,1.),.UNSPECIFIED.);
#471=B_SPLINE_CURVE_WITH_KNOTS('',3,(#12919,#12920,#12921,#12922),
 .UNSPECIFIED.,.F.,.F.,(4,4),(0.,1.),.UNSPECIFIED.);
#472=B_SPLINE_CURVE_WITH_KNOTS('',3,(#12924,#12925,#12926,#12927),
 .UNSPECIFIED.,.F.,.F.,(4,4),(0.,0.999999999984122),.UNSPECIFIED.);
#473=B_SPLINE_CURVE_WITH_KNOTS('',3,(#12931,#12932,#12933,#12934),
 .UNSPECIFIED.,.F.,.F.,(4,4),(0.,1.),.UNSPECIFIED.);
#474=B_SPLINE_CURVE_WITH_KNOTS('',3,(#12936,#12937,#12938,#12939),
 .UNSPECIFIED.,.F.,.F.,(4,4),(0.,0.999999999882221),.UNSPECIFIED.);
#475=B_SPLINE_CURVE_WITH_KNOTS('',3,(#12986,#12987,#12988,#12989,#12990,
#12991,#12992,#12993,#12994,#12995,#12996),.UNSPECIFIED.,.F.,.F.,(4,1,1,
1,1,1,1,1,4),(1.82133646569706E-10,0.125000000151206,0.250000000120279,
0.375000000089351,0.500000000058424,0.625000000027496,0.749999999996569,
0.874999999965641,0.999999999934714),.UNSPECIFIED.);
#476=B_SPLINE_CURVE_WITH_KNOTS('',3,(#13001,#13002,#13003,#13004,#13005,
#13006,#13007,#13008,#13009,#13010,#13011),.UNSPECIFIED.,.F.,.F.,(4,1,1,
1,1,1,1,1,4),(0.,0.125,0.25,0.375,0.5,0.625,0.75,0.875,1.),
 .UNSPECIFIED.);
#477=B_SPLINE_CURVE_WITH_KNOTS('',3,(#13016,#13017,#13018,#13019,#13020,
#13021,#13022),.UNSPECIFIED.,.F.,.F.,(4,1,1,1,4),(1.08159974291989E-10,
0.250000000064798,0.500000000021436,0.749999999978074,0.999999999934712),
 .UNSPECIFIED.);
#478=B_SPLINE_CURVE_WITH_KNOTS('',3,(#13030,#13031,#13032,#13033,#13034,
#13035,#13036),.UNSPECIFIED.,.F.,.F.,(4,1,1,1,4),(0.,0.25,0.5,0.75,1.),
 .UNSPECIFIED.);
#479=B_SPLINE_CURVE_WITH_KNOTS('',3,(#13044,#13045,#13046,#13047,#13048,
#13049,#13050,#13051,#13052,#13053,#13054),.UNSPECIFIED.,.F.,.F.,(4,1,1,
1,1,1,1,1,4),(4.32086807808983E-11,0.125000000029647,0.250000000016085,
0.375000000002522,0.49999999998896,0.624999999975398,0.749999999961836,
0.874999999948274,0.999999999934712),.UNSPECIFIED.);
#480=B_SPLINE_CURVE_WITH_KNOTS('',3,(#13056,#13057,#13058,#13059),
 .UNSPECIFIED.,.F.,.F.,(4,4),(0.,1.),.UNSPECIFIED.);
#481=B_SPLINE_CURVE_WITH_KNOTS('',3,(#13061,#13062,#13063,#13064,#13065,
#13066,#13067),.UNSPECIFIED.,.F.,.F.,(4,1,1,1,4),(6.52880993013389E-11,
0.250000000020525,0.499999999975762,0.749999999930999,0.999999999886236),
 .UNSPECIFIED.);
#482=B_SPLINE_CURVE_WITH_KNOTS('',3,(#13069,#13070,#13071,#13072),
 .UNSPECIFIED.,.F.,.F.,(4,4),(0.,1.),.UNSPECIFIED.);
#483=B_SPLINE_CURVE_WITH_KNOTS('',3,(#13076,#13077,#13078,#13079,#13080,
#13081,#13082,#13083,#13084,#13085,#13086),.UNSPECIFIED.,.F.,.F.,(4,1,1,
1,1,1,1,1,4),(0.,0.125,0.25,0.375,0.5,0.625,0.75,0.875,1.),
 .UNSPECIFIED.);
#484=B_SPLINE_CURVE_WITH_KNOTS('',3,(#13094,#13095,#13096,#13097,#13098,
#13099,#13100,#13101,#13102,#13103,#13104),.UNSPECIFIED.,.F.,.F.,(4,1,1,
1,1,1,1,1,4),(0.,0.125,0.25,0.375,0.5,0.625,0.75,0.875,1.),
 .UNSPECIFIED.);
#485=B_SPLINE_CURVE_WITH_KNOTS('',3,(#13106,#13107,#13108,#13109),
 .UNSPECIFIED.,.F.,.F.,(4,4),(0.,1.),.UNSPECIFIED.);
#486=B_SPLINE_CURVE_WITH_KNOTS('',3,(#13113,#13114,#13115,#13116),
 .UNSPECIFIED.,.F.,.F.,(4,4),(0.,1.),.UNSPECIFIED.);
#487=B_SPLINE_CURVE_WITH_KNOTS('',3,(#13118,#13119,#13120,#13121,#13122,
#13123,#13124,#13125,#13126,#13127,#13128),.UNSPECIFIED.,.F.,.F.,(4,1,1,
1,1,1,1,1,4),(6.52871450848788E-11,0.125000000057126,0.250000000048965,
0.375000000040805,0.500000000032644,0.625000000024483,0.750000000016322,
0.875000000008161,1.),.UNSPECIFIED.);
#488=B_SPLINE_CURVE_WITH_KNOTS('',3,(#13130,#13131,#13132,#13133),
 .UNSPECIFIED.,.F.,.F.,(4,4),(0.,1.),.UNSPECIFIED.);
#489=B_SPLINE_CURVE_WITH_KNOTS('',3,(#13135,#13136,#13137,#13138,#13139,
#13140,#13141,#13142,#13143,#13144,#13145),.UNSPECIFIED.,.F.,.F.,(4,1,1,
1,1,1,1,1,4),(7.9578112254039E-11,0.12500000006147,0.250000000043362,0.375000000025254,
0.500000000007146,0.624999999989038,0.74999999997093,0.874999999952822,
0.999999999934714),.UNSPECIFIED.);
#490=B_SPLINE_CURVE_WITH_KNOTS('',3,(#13147,#13148,#13149,#13150),
 .UNSPECIFIED.,.F.,.F.,(4,4),(0.,1.),.UNSPECIFIED.);
#491=B_SPLINE_CURVE_WITH_KNOTS('',3,(#13170,#13171,#13172,#13173,#13174,
#13175,#13176,#13177,#13178,#13179,#13180),.UNSPECIFIED.,.F.,.F.,(4,1,1,
1,1,1,1,1,4),(1.82133646569706E-10,0.125000000151206,0.250000000120279,
0.375000000089351,0.500000000058424,0.625000000027496,0.749999999996569,
0.874999999965641,0.999999999934714),.UNSPECIFIED.);
#492=B_SPLINE_CURVE_WITH_KNOTS('',3,(#13185,#13186,#13187,#13188,#13189,
#13190,#13191,#13192,#13193,#13194,#13195),.UNSPECIFIED.,.F.,.F.,(4,1,1,
1,1,1,1,1,4),(0.,0.125,0.25,0.375,0.5,0.625,0.75,0.875,1.),
 .UNSPECIFIED.);
#493=B_SPLINE_CURVE_WITH_KNOTS('',3,(#13200,#13201,#13202,#13203,#13204,
#13205,#13206),.UNSPECIFIED.,.F.,.F.,(4,1,1,1,4),(1.08159974291989E-10,
0.250000000064798,0.500000000021436,0.749999999978074,0.999999999934712),
 .UNSPECIFIED.);
#494=B_SPLINE_CURVE_WITH_KNOTS('',3,(#13214,#13215,#13216,#13217,#13218,
#13219,#13220),.UNSPECIFIED.,.F.,.F.,(4,1,1,1,4),(0.,0.25,0.5,0.75,1.),
 .UNSPECIFIED.);
#495=B_SPLINE_CURVE_WITH_KNOTS('',3,(#13228,#13229,#13230,#13231,#13232,
#13233,#13234,#13235,#13236,#13237,#13238),.UNSPECIFIED.,.F.,.F.,(4,1,1,
1,1,1,1,1,4),(4.32086807808983E-11,0.125000000029647,0.250000000016085,
0.375000000002522,0.49999999998896,0.624999999975398,0.749999999961836,
0.874999999948274,0.999999999934712),.UNSPECIFIED.);
#496=B_SPLINE_CURVE_WITH_KNOTS('',3,(#13240,#13241,#13242,#13243),
 .UNSPECIFIED.,.F.,.F.,(4,4),(0.,1.),.UNSPECIFIED.);
#497=B_SPLINE_CURVE_WITH_KNOTS('',3,(#13245,#13246,#13247,#13248,#13249,
#13250,#13251),.UNSPECIFIED.,.F.,.F.,(4,1,1,1,4),(6.52880993013389E-11,
0.250000000020525,0.499999999975762,0.749999999930999,0.999999999886236),
 .UNSPECIFIED.);
#498=B_SPLINE_CURVE_WITH_KNOTS('',3,(#13253,#13254,#13255,#13256),
 .UNSPECIFIED.,.F.,.F.,(4,4),(0.,1.),.UNSPECIFIED.);
#499=B_SPLINE_CURVE_WITH_KNOTS('',3,(#13260,#13261,#13262,#13263,#13264,
#13265,#13266,#13267,#13268,#13269,#13270),.UNSPECIFIED.,.F.,.F.,(4,1,1,
1,1,1,1,1,4),(0.,0.125,0.25,0.375,0.5,0.625,0.75,0.875,1.),
 .UNSPECIFIED.);
#500=B_SPLINE_CURVE_WITH_KNOTS('',3,(#13278,#13279,#13280,#13281,#13282,
#13283,#13284,#13285,#13286,#13287,#13288),.UNSPECIFIED.,.F.,.F.,(4,1,1,
1,1,1,1,1,4),(0.,0.125,0.25,0.375,0.5,0.625,0.75,0.875,1.),
 .UNSPECIFIED.);
#501=B_SPLINE_CURVE_WITH_KNOTS('',3,(#13290,#13291,#13292,#13293),
 .UNSPECIFIED.,.F.,.F.,(4,4),(0.,1.),.UNSPECIFIED.);
#502=B_SPLINE_CURVE_WITH_KNOTS('',3,(#13297,#13298,#13299,#13300),
 .UNSPECIFIED.,.F.,.F.,(4,4),(0.,1.),.UNSPECIFIED.);
#503=B_SPLINE_CURVE_WITH_KNOTS('',3,(#13302,#13303,#13304,#13305,#13306,
#13307,#13308,#13309,#13310,#13311,#13312),.UNSPECIFIED.,.F.,.F.,(4,1,1,
1,1,1,1,1,4),(6.52871450848788E-11,0.125000000057126,0.250000000048965,
0.375000000040805,0.500000000032644,0.625000000024483,0.750000000016322,
0.875000000008161,1.),.UNSPECIFIED.);
#504=B_SPLINE_CURVE_WITH_KNOTS('',3,(#13314,#13315,#13316,#13317),
 .UNSPECIFIED.,.F.,.F.,(4,4),(0.,1.),.UNSPECIFIED.);
#505=B_SPLINE_CURVE_WITH_KNOTS('',3,(#13319,#13320,#13321,#13322,#13323,
#13324,#13325,#13326,#13327,#13328,#13329),.UNSPECIFIED.,.F.,.F.,(4,1,1,
1,1,1,1,1,4),(7.9578112254039E-11,0.12500000006147,0.250000000043362,0.375000000025254,
0.500000000007146,0.624999999989038,0.74999999997093,0.874999999952822,
0.999999999934714),.UNSPECIFIED.);
#506=B_SPLINE_CURVE_WITH_KNOTS('',3,(#13331,#13332,#13333,#13334),
 .UNSPECIFIED.,.F.,.F.,(4,4),(0.,1.),.UNSPECIFIED.);
#507=B_SPLINE_CURVE_WITH_KNOTS('',3,(#13340,#13341,#13342,#13343,#13344,
#13345,#13346,#13347,#13348,#13349,#13350),.UNSPECIFIED.,.F.,.F.,(4,1,1,
1,1,1,1,1,4),(6.5285800070357E-11,0.125000000047178,0.25000000002907,0.375000000010962,
0.499999999992854,0.624999999974746,0.749999999956638,0.87499999993853,
0.999999999920422),.UNSPECIFIED.);
#508=B_SPLINE_CURVE_WITH_KNOTS('',3,(#13360,#13361,#13362,#13363,#13364,
#13365,#13366,#13367,#13368,#13369,#13370),.UNSPECIFIED.,.F.,.F.,(4,1,1,
1,1,1,1,1,4),(0.,0.125,0.25,0.375,0.5,0.625,0.75,0.875,1.),
 .UNSPECIFIED.);
#509=B_SPLINE_CURVE_WITH_KNOTS('',3,(#13375,#13376,#13377,#13378,#13379,
#13380,#13381,#13382,#13383,#13384,#13385),.UNSPECIFIED.,.F.,.F.,(4,1,1,
1,1,1,1,1,4),(0.,0.125,0.25,0.375,0.5,0.625,0.75,0.875,1.),
 .UNSPECIFIED.);
#510=B_SPLINE_CURVE_WITH_KNOTS('',3,(#13393,#13394,#13395,#13396,#13397),
 .UNSPECIFIED.,.F.,.F.,(4,1,4),(0.,0.499999978485393,0.999999956970785),
 .UNSPECIFIED.);
#511=B_SPLINE_CURVE_WITH_KNOTS('',3,(#13399,#13400,#13401,#13402,#13403,
#13404,#13405,#13406,#13407,#13408,#13409),.UNSPECIFIED.,.F.,.F.,(4,1,1,
1,1,1,1,1,4),(1.08159811971616E-10,0.125000000086479,0.250000000064798,
0.375000000043118,0.500000000021437,0.624999999999756,0.749999999978076,
0.874999999956395,0.999999999934714),.UNSPECIFIED.);
#512=B_SPLINE_CURVE_WITH_KNOTS('',3,(#13411,#13412,#13413,#13414,#13415),
 .UNSPECIFIED.,.F.,.F.,(4,1,4),(4.3029215375297E-8,0.49999997764101,0.999999912252804),
 .UNSPECIFIED.);
#513=B_SPLINE_CURVE_WITH_KNOTS('',3,(#13425,#13426,#13427,#13428,#13429,
#13430,#13431,#13432,#13433,#13434,#13435),.UNSPECIFIED.,.F.,.F.,(4,1,1,
1,1,1,1,1,4),(0.,0.125,0.25,0.375,0.5,0.625,0.75,0.875,1.),
 .UNSPECIFIED.);
#514=B_SPLINE_CURVE_WITH_KNOTS('',3,(#13445,#13446,#13447,#13448,#13449),
 .UNSPECIFIED.,.F.,.F.,(4,1,4),(2.91751359515211E-8,0.499999949957411,0.999999870739685),
 .UNSPECIFIED.);
#515=B_SPLINE_CURVE_WITH_KNOTS('',3,(#13451,#13452,#13453,#13454,#13455),
 .UNSPECIFIED.,.F.,.F.,(4,1,4),(0.,0.499999985412432,0.999999970824864),
 .UNSPECIFIED.);
#516=B_SPLINE_CURVE_WITH_KNOTS('',3,(#13457,#13458,#13459,#13460,#13461,
#13462,#13463,#13464,#13465,#13466,#13467),.UNSPECIFIED.,.F.,.F.,(4,1,1,
1,1,1,1,1,4),(2.37190894409548E-10,0.125000000203969,0.250000000170748,
0.375000000137526,0.500000000104304,0.625000000071083,0.750000000037861,
0.875000000004639,0.999999999971418),.UNSPECIFIED.);
#517=B_SPLINE_CURVE_WITH_KNOTS('',3,(#13471,#13472,#13473,#13474),
 .UNSPECIFIED.,.F.,.F.,(4,4),(0.,1.),.UNSPECIFIED.);
#518=B_SPLINE_CURVE_WITH_KNOTS('',3,(#13476,#13477,#13478,#13479),
 .UNSPECIFIED.,.F.,.F.,(4,4),(0.,1.),.UNSPECIFIED.);
#519=B_SPLINE_CURVE_WITH_KNOTS('',3,(#13481,#13482,#13483,#13484,#13485,
#13486,#13487),.UNSPECIFIED.,.F.,.F.,(4,1,1,1,4),(1.82135136395292E-10,
0.25000000012028,0.500000000058424,0.749999999996569,0.999999999934713),
 .UNSPECIFIED.);
#520=B_SPLINE_CURVE_WITH_KNOTS('',3,(#13494,#13495,#13496,#13497,#13498,
#13499,#13500),.UNSPECIFIED.,.F.,.F.,(4,1,1,1,4),(0.,0.25,0.5,0.75,1.),
 .UNSPECIFIED.);
#521=B_SPLINE_CURVE_WITH_KNOTS('',3,(#13510,#13511,#13512,#13513),
 .UNSPECIFIED.,.F.,.F.,(4,4),(0.,1.),.UNSPECIFIED.);
#522=B_SPLINE_CURVE_WITH_KNOTS('',3,(#13514,#13515,#13516,#13517),
 .UNSPECIFIED.,.F.,.F.,(4,4),(0.,1.),.UNSPECIFIED.);
#523=B_SPLINE_CURVE_WITH_KNOTS('',3,(#13521,#13522,#13523,#13524,#13525,
#13526,#13527,#13528,#13529,#13530,#13531),.UNSPECIFIED.,.F.,.F.,(4,1,1,
1,1,1,1,1,4),(6.5285800070357E-11,0.125000000047178,0.25000000002907,0.375000000010962,
0.499999999992854,0.624999999974746,0.749999999956638,0.87499999993853,
0.999999999920422),.UNSPECIFIED.);
#524=B_SPLINE_CURVE_WITH_KNOTS('',3,(#13541,#13542,#13543,#13544,#13545,
#13546,#13547,#13548,#13549,#13550,#13551),.UNSPECIFIED.,.F.,.F.,(4,1,1,
1,1,1,1,1,4),(0.,0.125,0.25,0.375,0.5,0.625,0.75,0.875,1.),
 .UNSPECIFIED.);
#525=B_SPLINE_CURVE_WITH_KNOTS('',3,(#13556,#13557,#13558,#13559,#13560,
#13561,#13562,#13563,#13564,#13565,#13566),.UNSPECIFIED.,.F.,.F.,(4,1,1,
1,1,1,1,1,4),(0.,0.125,0.25,0.375,0.5,0.625,0.75,0.875,1.),
 .UNSPECIFIED.);
#526=B_SPLINE_CURVE_WITH_KNOTS('',3,(#13574,#13575,#13576,#13577,#13578),
 .UNSPECIFIED.,.F.,.F.,(4,1,4),(0.,0.499999978485393,0.999999956970785),
 .UNSPECIFIED.);
#527=B_SPLINE_CURVE_WITH_KNOTS('',3,(#13580,#13581,#13582,#13583,#13584,
#13585,#13586,#13587,#13588,#13589,#13590),.UNSPECIFIED.,.F.,.F.,(4,1,1,
1,1,1,1,1,4),(1.08159811971616E-10,0.125000000086479,0.250000000064798,
0.375000000043118,0.500000000021437,0.624999999999756,0.749999999978076,
0.874999999956395,0.999999999934714),.UNSPECIFIED.);
#528=B_SPLINE_CURVE_WITH_KNOTS('',3,(#13592,#13593,#13594,#13595,#13596),
 .UNSPECIFIED.,.F.,.F.,(4,1,4),(4.3029215375297E-8,0.49999997764101,0.999999912252804),
 .UNSPECIFIED.);
#529=B_SPLINE_CURVE_WITH_KNOTS('',3,(#13606,#13607,#13608,#13609,#13610,
#13611,#13612,#13613,#13614,#13615,#13616),.UNSPECIFIED.,.F.,.F.,(4,1,1,
1,1,1,1,1,4),(0.,0.125,0.25,0.375,0.5,0.625,0.75,0.875,1.),
 .UNSPECIFIED.);
#530=B_SPLINE_CURVE_WITH_KNOTS('',3,(#13626,#13627,#13628,#13629,#13630),
 .UNSPECIFIED.,.F.,.F.,(4,1,4),(2.91751359515211E-8,0.499999949957411,0.999999870739685),
 .UNSPECIFIED.);
#531=B_SPLINE_CURVE_WITH_KNOTS('',3,(#13632,#13633,#13634,#13635,#13636),
 .UNSPECIFIED.,.F.,.F.,(4,1,4),(0.,0.499999985412432,0.999999970824864),
 .UNSPECIFIED.);
#532=B_SPLINE_CURVE_WITH_KNOTS('',3,(#13638,#13639,#13640,#13641,#13642,
#13643,#13644,#13645,#13646,#13647,#13648),.UNSPECIFIED.,.F.,.F.,(4,1,1,
1,1,1,1,1,4),(2.37190894409548E-10,0.125000000203969,0.250000000170748,
0.375000000137526,0.500000000104304,0.625000000071083,0.750000000037861,
0.875000000004639,0.999999999971418),.UNSPECIFIED.);
#533=B_SPLINE_CURVE_WITH_KNOTS('',3,(#13652,#13653,#13654,#13655),
 .UNSPECIFIED.,.F.,.F.,(4,4),(0.,1.),.UNSPECIFIED.);
#534=B_SPLINE_CURVE_WITH_KNOTS('',3,(#13657,#13658,#13659,#13660),
 .UNSPECIFIED.,.F.,.F.,(4,4),(0.,1.),.UNSPECIFIED.);
#535=B_SPLINE_CURVE_WITH_KNOTS('',3,(#13662,#13663,#13664,#13665,#13666,
#13667,#13668),.UNSPECIFIED.,.F.,.F.,(4,1,1,1,4),(1.82135136395292E-10,
0.25000000012028,0.500000000058424,0.749999999996569,0.999999999934713),
 .UNSPECIFIED.);
#536=B_SPLINE_CURVE_WITH_KNOTS('',3,(#13675,#13676,#13677,#13678,#13679,
#13680,#13681),.UNSPECIFIED.,.F.,.F.,(4,1,1,1,4),(0.,0.25,0.5,0.75,1.),
 .UNSPECIFIED.);
#537=B_SPLINE_CURVE_WITH_KNOTS('',3,(#13691,#13692,#13693,#13694),
 .UNSPECIFIED.,.F.,.F.,(4,4),(0.,1.),.UNSPECIFIED.);
#538=B_SPLINE_CURVE_WITH_KNOTS('',3,(#13695,#13696,#13697,#13698),
 .UNSPECIFIED.,.F.,.F.,(4,4),(0.,1.),.UNSPECIFIED.);
#539=B_SPLINE_CURVE_WITH_KNOTS('',3,(#13902,#13903,#13904,#13905,#13906,
#13907,#13908,#13909,#13910,#13911,#13912),.UNSPECIFIED.,.F.,.F.,(4,1,1,
1,1,1,1,1,4),(1.8213390095657E-10,0.125000000151206,0.250000000120279,0.375000000089351,
0.500000000058424,0.625000000027496,0.749999999996569,0.874999999965641,
0.999999999934714),.UNSPECIFIED.);
#540=B_SPLINE_CURVE_WITH_KNOTS('',3,(#13917,#13918,#13919,#13920,#13921,
#13922,#13923,#13924,#13925,#13926,#13927),.UNSPECIFIED.,.F.,.F.,(4,1,1,
1,1,1,1,1,4),(0.,0.124999999998599,0.249999999997198,0.374999999995797,
0.499999999994396,0.624999999992995,0.749999999991595,0.874999999990194,
0.999999999988793),.UNSPECIFIED.);
#541=B_SPLINE_CURVE_WITH_KNOTS('',3,(#13934,#13935,#13936,#13937,#13938,
#13939,#13940,#13941,#13942,#13943,#13944),.UNSPECIFIED.,.F.,.F.,(4,1,1,
1,1,1,1,1,4),(0.,0.125,0.25,0.375,0.5,0.625,0.75,0.875,1.),
 .UNSPECIFIED.);
#542=B_SPLINE_CURVE_WITH_KNOTS('',3,(#13952,#13953,#13954,#13955,#13956,
#13957,#13958,#13959,#13960,#13961,#13962),.UNSPECIFIED.,.F.,.F.,(4,1,1,
1,1,1,1,1,4),(0.,0.124999999998599,0.249999999997198,0.374999999995797,
0.499999999994396,0.624999999992995,0.749999999991595,0.874999999990194,
0.999999999988793),.UNSPECIFIED.);
#543=B_SPLINE_CURVE_WITH_KNOTS('',3,(#13964,#13965,#13966,#13967,#13968,
#13969,#13970,#13971,#13972,#13973,#13974),.UNSPECIFIED.,.F.,.F.,(4,1,1,
1,1,1,1,1,4),(0.,0.125,0.25,0.375,0.5,0.625,0.75,0.875,1.),
 .UNSPECIFIED.);
#544=B_SPLINE_CURVE_WITH_KNOTS('',3,(#13977,#13978,#13979,#13980,#13981,
#13982,#13983,#13984,#13985,#13986,#13987),.UNSPECIFIED.,.F.,.F.,(4,1,1,
1,1,1,1,1,4),(0.,0.125,0.25,0.375,0.5,0.625,0.75,0.875,1.),
 .UNSPECIFIED.);
#545=B_SPLINE_CURVE_WITH_KNOTS('',3,(#13993,#13994,#13995,#13996,#13997,
#13998,#13999,#14000,#14001,#14002,#14003),.UNSPECIFIED.,.F.,.F.,(4,1,1,
1,1,1,1,1,4),(0.,0.124999999995026,0.249999999990053,0.374999999985079,
0.499999999980106,0.624999999975132,0.749999999970159,0.874999999965185,
0.999999999960211),.UNSPECIFIED.);
#546=B_SPLINE_CURVE_WITH_KNOTS('',3,(#14011,#14012,#14013,#14014),
 .UNSPECIFIED.,.F.,.F.,(4,4),(0.,1.),.UNSPECIFIED.);
#547=B_SPLINE_CURVE_WITH_KNOTS('',3,(#14018,#14019,#14020,#14021),
 .UNSPECIFIED.,.F.,.F.,(4,4),(0.,1.),.UNSPECIFIED.);
#548=B_SPLINE_CURVE_WITH_KNOTS('',3,(#14023,#14024,#14025,#14026,#14027,
#14028,#14029,#14030,#14031,#14032,#14033),.UNSPECIFIED.,.F.,.F.,(4,1,1,
1,1,1,1,1,4),(6.52855121179665E-11,0.125000000057125,0.250000000048964,
0.375000000040804,0.500000000032643,0.625000000024482,0.750000000016322,
0.875000000008161,1.),.UNSPECIFIED.);
#549=B_SPLINE_CURVE_WITH_KNOTS('',3,(#14038,#14039,#14040,#14041,#14042,
#14043,#14044,#14045,#14046,#14047,#14048),.UNSPECIFIED.,.F.,.F.,(4,1,1,
1,1,1,1,1,4),(1.12066807818024E-11,0.125000000009806,0.250000000008405,
0.375000000007004,0.500000000005603,0.625000000004202,0.750000000002802,
0.875000000001401,1.),.UNSPECIFIED.);
#550=B_SPLINE_CURVE_WITH_KNOTS('',3,(#14050,#14051,#14052,#14053),
 .UNSPECIFIED.,.F.,.F.,(4,4),(-3.98872334206739E-9,1.),.UNSPECIFIED.);
#551=B_SPLINE_CURVE_WITH_KNOTS('',3,(#14056,#14057,#14058,#14059),
 .UNSPECIFIED.,.F.,.F.,(4,4),(0.,0.999999999803539),.UNSPECIFIED.);
#552=B_SPLINE_CURVE_WITH_KNOTS('',3,(#14061,#14062,#14063,#14064,#14065,
#14066,#14067,#14068,#14069,#14070),.UNSPECIFIED.,.F.,.F.,(4,1,1,1,1,1,
1,4),(0.,0.25,0.375,0.5,0.5625,0.625,0.75,1.),.UNSPECIFIED.);
#553=B_SPLINE_CURVE_WITH_KNOTS('',3,(#14072,#14073,#14074,#14075),
 .UNSPECIFIED.,.F.,.F.,(4,4),(0.,1.),.UNSPECIFIED.);
#554=B_SPLINE_CURVE_WITH_KNOTS('',3,(#14077,#14078,#14079,#14080,#14081,
#14082,#14083,#14084,#14085,#14086),.UNSPECIFIED.,.F.,.F.,(4,1,1,1,1,1,
1,4),(0.,0.25,0.375,0.4375,0.5,0.625,0.75,1.),.UNSPECIFIED.);
#555=B_SPLINE_CURVE_WITH_KNOTS('',3,(#14088,#14089,#14090,#14091),
 .UNSPECIFIED.,.F.,.F.,(4,4),(0.,1.),.UNSPECIFIED.);
#556=B_SPLINE_CURVE_WITH_KNOTS('',3,(#14093,#14094,#14095,#14096,#14097,
#14098,#14099,#14100,#14101,#14102),.UNSPECIFIED.,.F.,.F.,(4,1,1,1,1,1,
1,4),(0.,0.25,0.375,0.5,0.5625,0.625,0.75,1.),.UNSPECIFIED.);
#557=B_SPLINE_CURVE_WITH_KNOTS('',3,(#14104,#14105,#14106,#14107),
 .UNSPECIFIED.,.F.,.F.,(4,4),(0.,1.),.UNSPECIFIED.);
#558=B_SPLINE_CURVE_WITH_KNOTS('',3,(#14109,#14110,#14111,#14112,#14113,
#14114,#14115,#14116,#14117,#14118),.UNSPECIFIED.,.F.,.F.,(4,1,1,1,1,1,
1,4),(0.,0.25,0.375,0.4375,0.5,0.625,0.75,1.),.UNSPECIFIED.);
#559=B_SPLINE_CURVE_WITH_KNOTS('',3,(#14120,#14121,#14122,#14123),
 .UNSPECIFIED.,.F.,.F.,(4,4),(0.,1.),.UNSPECIFIED.);
#560=B_SPLINE_CURVE_WITH_KNOTS('',3,(#14125,#14126,#14127,#14128,#14129,
#14130,#14131,#14132,#14133,#14134),.UNSPECIFIED.,.F.,.F.,(4,1,1,1,1,1,
1,4),(0.,0.25,0.375,0.5,0.5625,0.625,0.75,1.),.UNSPECIFIED.);
#561=B_SPLINE_CURVE_WITH_KNOTS('',3,(#14136,#14137,#14138,#14139),
 .UNSPECIFIED.,.F.,.F.,(4,4),(0.,1.),.UNSPECIFIED.);
#562=B_SPLINE_CURVE_WITH_KNOTS('',3,(#14141,#14142,#14143,#14144,#14145,
#14146,#14147,#14148,#14149,#14150),.UNSPECIFIED.,.F.,.F.,(4,1,1,1,1,1,
1,4),(0.,0.25,0.375,0.4375,0.5,0.625,0.75,1.),.UNSPECIFIED.);
#563=B_SPLINE_CURVE_WITH_KNOTS('',3,(#14154,#14155,#14156,#14157),
 .UNSPECIFIED.,.F.,.F.,(4,4),(0.,1.),.UNSPECIFIED.);
#564=B_SPLINE_CURVE_WITH_KNOTS('',3,(#14159,#14160,#14161,#14162,#14163,
#14164,#14165,#14166,#14167,#14168),.UNSPECIFIED.,.F.,.F.,(4,1,1,1,1,1,
1,4),(0.,0.25,0.375,0.5,0.5625,0.625,0.75,1.),.UNSPECIFIED.);
#565=B_SPLINE_CURVE_WITH_KNOTS('',3,(#14170,#14171,#14172,#14173),
 .UNSPECIFIED.,.F.,.F.,(4,4),(0.,1.),.UNSPECIFIED.);
#566=B_SPLINE_CURVE_WITH_KNOTS('',3,(#14175,#14176,#14177,#14178,#14179,
#14180,#14181,#14182,#14183,#14184),.UNSPECIFIED.,.F.,.F.,(4,1,1,1,1,1,
1,4),(0.,0.25,0.375,0.4375,0.5,0.625,0.75,1.),.UNSPECIFIED.);
#567=B_SPLINE_CURVE_WITH_KNOTS('',3,(#14186,#14187,#14188,#14189),
 .UNSPECIFIED.,.F.,.F.,(4,4),(0.,1.),.UNSPECIFIED.);
#568=B_SPLINE_CURVE_WITH_KNOTS('',3,(#14191,#14192,#14193,#14194,#14195,
#14196,#14197,#14198,#14199,#14200),.UNSPECIFIED.,.F.,.F.,(4,1,1,1,1,1,
1,4),(0.,0.25,0.375,0.5,0.5625,0.625,0.75,1.),.UNSPECIFIED.);
#569=B_SPLINE_CURVE_WITH_KNOTS('',3,(#14204,#14205,#14206,#14207,#14208,
#14209,#14210,#14211,#14212,#14213),.UNSPECIFIED.,.F.,.F.,(4,1,1,1,1,1,
1,4),(0.,0.25,0.375,0.4375,0.5,0.625,0.75,1.),.UNSPECIFIED.);
#570=B_SPLINE_CURVE_WITH_KNOTS('',3,(#14215,#14216,#14217,#14218),
 .UNSPECIFIED.,.F.,.F.,(4,4),(0.,1.),.UNSPECIFIED.);
#571=B_SPLINE_CURVE_WITH_KNOTS('',3,(#14220,#14221,#14222,#14223,#14224,
#14225,#14226,#14227,#14228,#14229),.UNSPECIFIED.,.F.,.F.,(4,1,1,1,1,1,
1,4),(0.,0.25,0.375,0.5,0.5625,0.625,0.75,1.),.UNSPECIFIED.);
#572=B_SPLINE_CURVE_WITH_KNOTS('',3,(#14231,#14232,#14233,#14234),
 .UNSPECIFIED.,.F.,.F.,(4,4),(0.,1.),.UNSPECIFIED.);
#573=B_SPLINE_CURVE_WITH_KNOTS('',3,(#14236,#14237,#14238,#14239,#14240,
#14241,#14242,#14243,#14244,#14245),.UNSPECIFIED.,.F.,.F.,(4,1,1,1,1,1,
1,4),(0.,0.25,0.375,0.4375,0.5,0.625,0.75,1.),.UNSPECIFIED.);
#574=B_SPLINE_CURVE_WITH_KNOTS('',3,(#14253,#14254,#14255,#14256,#14257,
#14258,#14259,#14260,#14261,#14262,#14263,#14264),.UNSPECIFIED.,.F.,.F.,
(4,1,1,1,1,1,1,1,1,4),(0.,0.25,0.5,0.625,0.75,0.8125,0.875,0.9375,0.96875,
1.),.UNSPECIFIED.);
#575=B_SPLINE_CURVE_WITH_KNOTS('',3,(#14265,#14266,#14267,#14268,#14269,
#14270,#14271,#14272,#14273,#14274,#14275,#14276,#14277),.UNSPECIFIED.,
 .F.,.F.,(4,1,1,1,1,1,1,1,1,1,4),(0.,0.015625,0.03125,0.0625,0.125,0.1875,
0.25,0.375,0.5,0.75,1.),.UNSPECIFIED.);
#576=B_SPLINE_CURVE_WITH_KNOTS('',3,(#14279,#14280,#14281,#14282),
 .UNSPECIFIED.,.F.,.F.,(4,4),(-0.000951209283696458,0.00026784888500917),
 .UNSPECIFIED.);
#577=B_SPLINE_CURVE_WITH_KNOTS('',3,(#14284,#14285,#14286,#14287,#14288),
 .UNSPECIFIED.,.F.,.F.,(4,1,4),(0.,0.499999854922505,0.99999970984501),
 .UNSPECIFIED.);
#578=B_SPLINE_CURVE_WITH_KNOTS('',3,(#14292,#14293,#14294,#14295,#14296),
 .UNSPECIFIED.,.F.,.F.,(4,1,4),(2.901447796702E-7,0.50000014507239,1.),
 .UNSPECIFIED.);
#579=B_SPLINE_CURVE_WITH_KNOTS('',3,(#14298,#14299,#14300,#14301),
 .UNSPECIFIED.,.F.,.F.,(4,4),(0.,0.00120725234162079),.UNSPECIFIED.);
#580=B_SPLINE_CURVE_WITH_KNOTS('',3,(#14303,#14304,#14305,#14306,#14307,
#14308,#14309,#14310,#14311,#14312,#14313,#14314,#14315),.UNSPECIFIED.,
 .F.,.F.,(4,1,1,1,1,1,1,1,1,1,4),(0.,0.015625,0.03125,0.0625,0.125,0.1875,
0.25,0.375,0.5,0.75,1.),.UNSPECIFIED.);
#581=B_SPLINE_CURVE_WITH_KNOTS('',3,(#14317,#14318,#14319,#14320),
 .UNSPECIFIED.,.F.,.F.,(4,4),(0.,1.),.UNSPECIFIED.);
#582=B_SPLINE_CURVE_WITH_KNOTS('',3,(#14322,#14323,#14324,#14325,#14326,
#14327,#14328,#14329,#14330,#14331,#14332,#14333),.UNSPECIFIED.,.F.,.F.,
(4,1,1,1,1,1,1,1,1,4),(0.,0.25,0.5,0.625,0.75,0.8125,0.875,0.9375,0.96875,
1.),.UNSPECIFIED.);
#583=B_SPLINE_CURVE_WITH_KNOTS('',3,(#14335,#14336,#14337,#14338),
 .UNSPECIFIED.,.F.,.F.,(4,4),(0.,0.00120749967935418),.UNSPECIFIED.);
#584=B_SPLINE_CURVE_WITH_KNOTS('',3,(#14340,#14341,#14342,#14343,#14344),
 .UNSPECIFIED.,.F.,.F.,(4,1,4),(0.,0.499999854925028,0.999999709850055),
 .UNSPECIFIED.);
#585=B_SPLINE_CURVE_WITH_KNOTS('',3,(#14348,#14349,#14350,#14351,#14352),
 .UNSPECIFIED.,.F.,.F.,(4,1,4),(2.90144772198091E-7,0.500000145072386,1.),
 .UNSPECIFIED.);
#586=B_SPLINE_CURVE_WITH_KNOTS('',3,(#14354,#14355,#14356,#14357),
 .UNSPECIFIED.,.F.,.F.,(4,4),(0.,0.00120725233944049),.UNSPECIFIED.);
#587=B_SPLINE_CURVE_WITH_KNOTS('',3,(#14359,#14360,#14361,#14362,#14363,
#14364,#14365,#14366,#14367,#14368,#14369,#14370,#14371),.UNSPECIFIED.,
 .F.,.F.,(4,1,1,1,1,1,1,1,1,1,4),(0.,0.015625,0.03125,0.0625,0.125,0.1875,
0.25,0.375,0.5,0.75,1.),.UNSPECIFIED.);
#588=B_SPLINE_CURVE_WITH_KNOTS('',3,(#14373,#14374,#14375,#14376),
 .UNSPECIFIED.,.F.,.F.,(4,4),(0.,1.),.UNSPECIFIED.);
#589=B_SPLINE_CURVE_WITH_KNOTS('',3,(#14378,#14379,#14380,#14381,#14382,
#14383,#14384,#14385,#14386,#14387,#14388,#14389),.UNSPECIFIED.,.F.,.F.,
(4,1,1,1,1,1,1,1,1,4),(0.,0.25,0.5,0.625,0.75,0.8125,0.875,0.9375,0.96875,
1.),.UNSPECIFIED.);
#590=B_SPLINE_CURVE_WITH_KNOTS('',3,(#14391,#14392,#14393,#14394),
 .UNSPECIFIED.,.F.,.F.,(4,4),(0.,0.00120749968240849),.UNSPECIFIED.);
#591=B_SPLINE_CURVE_WITH_KNOTS('',3,(#14396,#14397,#14398,#14399,#14400),
 .UNSPECIFIED.,.F.,.F.,(4,1,4),(0.,0.499999854925025,0.999999709850049),
 .UNSPECIFIED.);
#592=B_SPLINE_CURVE_WITH_KNOTS('',3,(#14404,#14405,#14406,#14407,#14408),
 .UNSPECIFIED.,.F.,.F.,(4,1,4),(2.901447750701E-7,0.500000145072388,1.),
 .UNSPECIFIED.);
#593=B_SPLINE_CURVE_WITH_KNOTS('',3,(#14410,#14411,#14412,#14413),
 .UNSPECIFIED.,.F.,.F.,(4,4),(0.,0.00120725234168436),.UNSPECIFIED.);
#594=B_SPLINE_CURVE_WITH_KNOTS('',3,(#14415,#14416,#14417,#14418,#14419),
 .UNSPECIFIED.,.F.,.F.,(4,1,4),(0.,0.5,1.),.UNSPECIFIED.);
#595=B_SPLINE_CURVE_WITH_KNOTS('',3,(#14421,#14422,#14423,#14424),
 .UNSPECIFIED.,.F.,.F.,(4,4),(-1.1112351980909E-15,1.),.UNSPECIFIED.);
#596=B_SPLINE_CURVE_WITH_KNOTS('',3,(#14428,#14429,#14430,#14431),
 .UNSPECIFIED.,.F.,.F.,(4,4),(0.,1.),.UNSPECIFIED.);
#597=B_SPLINE_CURVE_WITH_KNOTS('',3,(#14433,#14434,#14435,#14436,#14437),
 .UNSPECIFIED.,.F.,.F.,(4,1,4),(0.,0.5,1.),.UNSPECIFIED.);
#598=B_SPLINE_CURVE_WITH_KNOTS('',3,(#14439,#14440,#14441,#14442),
 .UNSPECIFIED.,.F.,.F.,(4,4),(0.,0.00120749968217001),.UNSPECIFIED.);
#599=B_SPLINE_CURVE_WITH_KNOTS('',3,(#14444,#14445,#14446,#14447,#14448),
 .UNSPECIFIED.,.F.,.F.,(4,1,4),(0.,0.49999985492503,0.999999709850059),
 .UNSPECIFIED.);
#600=B_SPLINE_CURVE_WITH_KNOTS('',3,(#14452,#14453,#14454,#14455,#14456),
 .UNSPECIFIED.,.F.,.F.,(4,1,4),(2.9014478282069E-7,0.500000145072391,1.),
 .UNSPECIFIED.);
#601=B_SPLINE_CURVE_WITH_KNOTS('',3,(#14458,#14459,#14460,#14461),
 .UNSPECIFIED.,.F.,.F.,(4,4),(0.,0.00120725234193258),.UNSPECIFIED.);
#602=B_SPLINE_CURVE_WITH_KNOTS('',3,(#14463,#14464,#14465,#14466,#14467),
 .UNSPECIFIED.,.F.,.F.,(4,1,4),(0.,0.5,1.),.UNSPECIFIED.);
#603=B_SPLINE_CURVE_WITH_KNOTS('',3,(#14469,#14470,#14471,#14472),
 .UNSPECIFIED.,.F.,.F.,(4,4),(0.,1.),.UNSPECIFIED.);
#604=B_SPLINE_CURVE_WITH_KNOTS('',3,(#14474,#14475,#14476,#14477,#14478),
 .UNSPECIFIED.,.F.,.F.,(4,1,4),(0.,0.5,1.),.UNSPECIFIED.);
#605=B_SPLINE_CURVE_WITH_KNOTS('',3,(#14480,#14481,#14482,#14483),
 .UNSPECIFIED.,.F.,.F.,(4,4),(0.,0.00120749968043747),.UNSPECIFIED.);
#606=B_SPLINE_CURVE_WITH_KNOTS('',3,(#14485,#14486,#14487,#14488,#14489),
 .UNSPECIFIED.,.F.,.F.,(4,1,4),(0.,0.499999854925027,0.999999709850054),
 .UNSPECIFIED.);
#607=B_SPLINE_CURVE_WITH_KNOTS('',3,(#14493,#14494,#14495,#14496,#14497),
 .UNSPECIFIED.,.F.,.F.,(4,1,4),(2.90144768683264E-7,0.500000145072384,1.),
 .UNSPECIFIED.);
#608=B_SPLINE_CURVE_WITH_KNOTS('',3,(#14499,#14500,#14501,#14502),
 .UNSPECIFIED.,.F.,.F.,(4,4),(0.,0.00120725233951242),.UNSPECIFIED.);
#609=B_SPLINE_CURVE_WITH_KNOTS('',3,(#14504,#14505,#14506,#14507,#14508),
 .UNSPECIFIED.,.F.,.F.,(4,1,4),(0.,0.5,1.),.UNSPECIFIED.);
#610=B_SPLINE_CURVE_WITH_KNOTS('',3,(#14510,#14511,#14512,#14513),
 .UNSPECIFIED.,.F.,.F.,(4,4),(0.,1.),.UNSPECIFIED.);
#611=B_SPLINE_CURVE_WITH_KNOTS('',3,(#14515,#14516,#14517,#14518,#14519),
 .UNSPECIFIED.,.F.,.F.,(4,1,4),(0.,0.5,1.),.UNSPECIFIED.);
#612=B_SPLINE_CURVE_WITH_KNOTS('',3,(#14521,#14522,#14523,#14524),
 .UNSPECIFIED.,.F.,.F.,(4,4),(0.,0.00120749968120778),.UNSPECIFIED.);
#613=B_SPLINE_CURVE_WITH_KNOTS('',3,(#14526,#14527,#14528,#14529,#14530),
 .UNSPECIFIED.,.F.,.F.,(4,1,4),(0.,0.499999854925025,0.999999709850049),
 .UNSPECIFIED.);
#614=B_SPLINE_CURVE_WITH_KNOTS('',3,(#14534,#14535,#14536,#14537,#14538),
 .UNSPECIFIED.,.F.,.F.,(4,1,4),(2.90149859374016E-7,0.50000014507493,1.),
 .UNSPECIFIED.);
#615=B_SPLINE_CURVE_WITH_KNOTS('',3,(#14540,#14541,#14542,#14543),
 .UNSPECIFIED.,.F.,.F.,(4,4),(-0.000265114428389933,0.000941618287195232),
 .UNSPECIFIED.);
#616=B_SPLINE_CURVE_WITH_KNOTS('',3,(#14548,#14549,#14550,#14551),
 .UNSPECIFIED.,.F.,.F.,(4,4),(0.,1.00000004166667),.UNSPECIFIED.);
#617=B_SPLINE_CURVE_WITH_KNOTS('',3,(#14553,#14554,#14555,#14556),
 .UNSPECIFIED.,.F.,.F.,(4,4),(-8.33333471783616E-8,1.),.UNSPECIFIED.);
#618=B_SPLINE_CURVE_WITH_KNOTS('',3,(#14562,#14563,#14564,#14565),
 .UNSPECIFIED.,.F.,.F.,(4,4),(0.,1.),.UNSPECIFIED.);
#619=B_SPLINE_CURVE_WITH_KNOTS('',3,(#14571,#14572,#14573,#14574),
 .UNSPECIFIED.,.F.,.F.,(4,4),(0.,1.),.UNSPECIFIED.);
#620=B_SPLINE_CURVE_WITH_KNOTS('',3,(#14580,#14581,#14582,#14583),
 .UNSPECIFIED.,.F.,.F.,(4,4),(0.,0.99999934647141),.UNSPECIFIED.);
#621=B_SPLINE_CURVE_WITH_KNOTS('',3,(#14591,#14592,#14593,#14594),
 .UNSPECIFIED.,.F.,.F.,(4,4),(0.,1.),.UNSPECIFIED.);
#622=B_SPLINE_CURVE_WITH_KNOTS('',3,(#14599,#14600,#14601,#14602),
 .UNSPECIFIED.,.F.,.F.,(4,4),(0.,0.999999345689277),.UNSPECIFIED.);
#623=B_SPLINE_CURVE_WITH_KNOTS('',3,(#14610,#14611,#14612,#14613),
 .UNSPECIFIED.,.F.,.F.,(4,4),(0.,1.),.UNSPECIFIED.);
#624=B_SPLINE_CURVE_WITH_KNOTS('',3,(#14616,#14617,#14618,#14619),
 .UNSPECIFIED.,.F.,.F.,(4,4),(0.,0.999999342822145),.UNSPECIFIED.);
#625=B_SPLINE_CURVE_WITH_KNOTS('',3,(#14627,#14628,#14629,#14630),
 .UNSPECIFIED.,.F.,.F.,(4,4),(0.,1.),.UNSPECIFIED.);
#626=B_SPLINE_CURVE_WITH_KNOTS('',3,(#14635,#14636,#14637,#14638),
 .UNSPECIFIED.,.F.,.F.,(4,4),(0.,0.999999346375954),.UNSPECIFIED.);
#627=B_SPLINE_CURVE_WITH_KNOTS('',3,(#14646,#14647,#14648,#14649),
 .UNSPECIFIED.,.F.,.F.,(4,4),(0.,1.),.UNSPECIFIED.);
#628=B_SPLINE_CURVE_WITH_KNOTS('',3,(#14654,#14655,#14656,#14657),
 .UNSPECIFIED.,.F.,.F.,(4,4),(0.,0.999999345593822),.UNSPECIFIED.);
#629=B_SPLINE_CURVE_WITH_KNOTS('',3,(#14665,#14666,#14667,#14668),
 .UNSPECIFIED.,.F.,.F.,(4,4),(0.,1.),.UNSPECIFIED.);
#630=B_SPLINE_CURVE_WITH_KNOTS('',3,(#14673,#14674,#14675,#14676),
 .UNSPECIFIED.,.F.,.F.,(4,4),(0.,0.999999342715313),.UNSPECIFIED.);
#631=B_SPLINE_CURVE_WITH_KNOTS('',3,(#14720,#14721,#14722,#14723),
 .UNSPECIFIED.,.F.,.F.,(4,4),(0.,1.),.UNSPECIFIED.);
#632=B_SPLINE_CURVE_WITH_KNOTS('',3,(#14727,#14728,#14729,#14730),
 .UNSPECIFIED.,.F.,.F.,(4,4),(-4.16666747456633E-8,1.),.UNSPECIFIED.);
#633=B_SPLINE_CURVE_WITH_KNOTS('',3,(#14732,#14733,#14734,#14735),
 .UNSPECIFIED.,.F.,.F.,(4,4),(0.,1.00000004166667),.UNSPECIFIED.);
#634=B_SPLINE_CURVE_WITH_KNOTS('',3,(#14741,#14742,#14743,#14744),
 .UNSPECIFIED.,.F.,.F.,(4,4),(0.,1.),.UNSPECIFIED.);
#635=B_SPLINE_CURVE_WITH_KNOTS('',3,(#14746,#14747,#14748,#14749),
 .UNSPECIFIED.,.F.,.F.,(4,4),(0.,1.),.UNSPECIFIED.);
#636=B_SPLINE_CURVE_WITH_KNOTS('',3,(#14753,#14754,#14755,#14756),
 .UNSPECIFIED.,.F.,.F.,(4,4),(-4.16666735891808E-8,1.),.UNSPECIFIED.);
#637=B_SPLINE_CURVE_WITH_KNOTS('',3,(#14760,#14761,#14762,#14763),
 .UNSPECIFIED.,.F.,.F.,(4,4),(0.,1.00000004166667),.UNSPECIFIED.);
#638=B_SPLINE_CURVE_WITH_KNOTS('',3,(#14767,#14768,#14769,#14770),
 .UNSPECIFIED.,.F.,.F.,(4,4),(0.,1.),.UNSPECIFIED.);
#639=B_SPLINE_CURVE_WITH_KNOTS('',3,(#14772,#14773,#14774,#14775),
 .UNSPECIFIED.,.F.,.F.,(4,4),(0.,1.),.UNSPECIFIED.);
#640=B_SPLINE_CURVE_WITH_KNOTS('',3,(#14779,#14780,#14781,#14782),
 .UNSPECIFIED.,.F.,.F.,(4,4),(-4.16666735891808E-8,1.),.UNSPECIFIED.);
#641=B_SPLINE_CURVE_WITH_KNOTS('',3,(#14786,#14787,#14788,#14789),
 .UNSPECIFIED.,.F.,.F.,(4,4),(0.,1.00000004166667),.UNSPECIFIED.);
#642=B_SPLINE_CURVE_WITH_KNOTS('',3,(#14793,#14794,#14795,#14796),
 .UNSPECIFIED.,.F.,.F.,(4,4),(0.,1.),.UNSPECIFIED.);
#643=B_SPLINE_CURVE_WITH_KNOTS('',3,(#14798,#14799,#14800,#14801),
 .UNSPECIFIED.,.F.,.F.,(4,4),(0.,1.),.UNSPECIFIED.);
#644=B_SPLINE_CURVE_WITH_KNOTS('',3,(#14805,#14806,#14807,#14808),
 .UNSPECIFIED.,.F.,.F.,(4,4),(-4.16666747456633E-8,1.),.UNSPECIFIED.);
#645=B_SPLINE_CURVE_WITH_KNOTS('',3,(#14812,#14813,#14814,#14815),
 .UNSPECIFIED.,.F.,.F.,(4,4),(0.,1.00000004166667),.UNSPECIFIED.);
#646=B_SPLINE_CURVE_WITH_KNOTS('',3,(#14819,#14820,#14821,#14822),
 .UNSPECIFIED.,.F.,.F.,(4,4),(0.,1.),.UNSPECIFIED.);
#647=B_SPLINE_CURVE_WITH_KNOTS('',3,(#14824,#14825,#14826,#14827),
 .UNSPECIFIED.,.F.,.F.,(4,4),(0.,1.),.UNSPECIFIED.);
#648=B_SPLINE_CURVE_WITH_KNOTS('',3,(#14831,#14832,#14833,#14834),
 .UNSPECIFIED.,.F.,.F.,(4,4),(-4.16666735891808E-8,1.),.UNSPECIFIED.);
#649=B_SPLINE_CURVE_WITH_KNOTS('',3,(#14836,#14837,#14838,#14839),
 .UNSPECIFIED.,.F.,.F.,(4,4),(0.,1.00000004166667),.UNSPECIFIED.);
#650=B_SPLINE_CURVE_WITH_KNOTS('',3,(#14845,#14846,#14847,#14848),
 .UNSPECIFIED.,.F.,.F.,(4,4),(0.,1.),.UNSPECIFIED.);
#651=B_SPLINE_CURVE_WITH_KNOTS('',3,(#14852,#14853,#14854,#14855),
 .UNSPECIFIED.,.F.,.F.,(4,4),(0.,1.),.UNSPECIFIED.);
#652=B_SPLINE_CURVE_WITH_KNOTS('',3,(#14860,#14861,#14862,#14863,#14864,
#14865,#14866,#14867,#14868,#14869,#14870),.UNSPECIFIED.,.F.,.F.,(4,1,1,
1,1,1,1,1,4),(2.37189194415179E-10,0.125000000203968,0.250000000170747,
0.375000000137525,0.500000000104304,0.625000000071083,0.750000000037861,
0.87500000000464,0.999999999971419),.UNSPECIFIED.);
#653=B_SPLINE_CURVE_WITH_KNOTS('',3,(#14879,#14880,#14881,#14882),
 .UNSPECIFIED.,.F.,.F.,(4,4),(0.,0.999999613428237),.UNSPECIFIED.);
#654=B_SPLINE_CURVE_WITH_KNOTS('',3,(#14883,#14884,#14885,#14886),
 .UNSPECIFIED.,.F.,.F.,(4,4),(0.,1.),.UNSPECIFIED.);
#655=B_SPLINE_CURVE_WITH_KNOTS('',3,(#14891,#14892,#14893,#14894),
 .UNSPECIFIED.,.F.,.F.,(4,4),(0.,1.),.UNSPECIFIED.);
#656=B_SPLINE_CURVE_WITH_KNOTS('',3,(#14902,#14903,#14904,#14905),
 .UNSPECIFIED.,.F.,.F.,(4,4),(0.,1.),.UNSPECIFIED.);
#657=B_SPLINE_CURVE_WITH_KNOTS('',3,(#14906,#14907,#14908,#14909),
 .UNSPECIFIED.,.F.,.F.,(4,4),(0.,1.),.UNSPECIFIED.);
#658=B_SPLINE_CURVE_WITH_KNOTS('',3,(#14917,#14918,#14919,#14920),
 .UNSPECIFIED.,.F.,.F.,(4,4),(0.,1.),.UNSPECIFIED.);
#659=B_SPLINE_CURVE_WITH_KNOTS('',3,(#14921,#14922,#14923,#14924),
 .UNSPECIFIED.,.F.,.F.,(4,4),(0.,1.),.UNSPECIFIED.);
#660=B_SPLINE_CURVE_WITH_KNOTS('',3,(#14932,#14933,#14934,#14935),
 .UNSPECIFIED.,.F.,.F.,(4,4),(0.,1.),.UNSPECIFIED.);
#661=B_SPLINE_CURVE_WITH_KNOTS('',3,(#14936,#14937,#14938,#14939),
 .UNSPECIFIED.,.F.,.F.,(4,4),(0.,1.),.UNSPECIFIED.);
#662=B_SPLINE_CURVE_WITH_KNOTS('',3,(#14947,#14948,#14949,#14950),
 .UNSPECIFIED.,.F.,.F.,(4,4),(0.,1.),.UNSPECIFIED.);
#663=B_SPLINE_CURVE_WITH_KNOTS('',3,(#14954,#14955,#14956,#14957),
 .UNSPECIFIED.,.F.,.F.,(4,4),(0.,1.),.UNSPECIFIED.);
#664=B_SPLINE_CURVE_WITH_KNOTS('',3,(#14958,#14959,#14960,#14961),
 .UNSPECIFIED.,.F.,.F.,(4,4),(0.,1.),.UNSPECIFIED.);
#665=B_SPLINE_CURVE_WITH_KNOTS('',3,(#15003,#15004,#15005,#15006),
 .UNSPECIFIED.,.F.,.F.,(4,4),(4.16666666447352E-8,1.),.UNSPECIFIED.);
#666=B_SPLINE_CURVE_WITH_KNOTS('',3,(#15026,#15027,#15028,#15029),
 .UNSPECIFIED.,.F.,.F.,(4,4),(4.16666666447352E-8,1.),.UNSPECIFIED.);
#667=B_SPLINE_CURVE_WITH_KNOTS('',3,(#15031,#15032,#15033,#15034),
 .UNSPECIFIED.,.F.,.F.,(4,4),(0.,1.),.UNSPECIFIED.);
#668=B_SPLINE_CURVE_WITH_KNOTS('',3,(#15036,#15037,#15038,#15039),
 .UNSPECIFIED.,.F.,.F.,(4,4),(0.,1.),.UNSPECIFIED.);
#669=B_SPLINE_CURVE_WITH_KNOTS('',3,(#15041,#15042,#15043,#15044),
 .UNSPECIFIED.,.F.,.F.,(4,4),(0.,1.),.UNSPECIFIED.);
#670=B_SPLINE_CURVE_WITH_KNOTS('',3,(#15047,#15048,#15049,#15050),
 .UNSPECIFIED.,.F.,.F.,(4,4),(4.16666666447351E-8,1.),.UNSPECIFIED.);
#671=B_SPLINE_CURVE_WITH_KNOTS('',3,(#15052,#15053,#15054,#15055),
 .UNSPECIFIED.,.F.,.F.,(4,4),(0.,1.),.UNSPECIFIED.);
#672=B_SPLINE_CURVE_WITH_KNOTS('',3,(#15057,#15058,#15059,#15060),
 .UNSPECIFIED.,.F.,.F.,(4,4),(0.,1.),.UNSPECIFIED.);
#673=B_SPLINE_CURVE_WITH_KNOTS('',3,(#15062,#15063,#15064,#15065),
 .UNSPECIFIED.,.F.,.F.,(4,4),(0.,1.),.UNSPECIFIED.);
#674=B_SPLINE_CURVE_WITH_KNOTS('',3,(#15068,#15069,#15070,#15071),
 .UNSPECIFIED.,.F.,.F.,(4,4),(0.,1.),.UNSPECIFIED.);
#675=B_SPLINE_CURVE_WITH_KNOTS('',3,(#15073,#15074,#15075,#15076),
 .UNSPECIFIED.,.F.,.F.,(4,4),(0.,1.),.UNSPECIFIED.);
#676=B_SPLINE_CURVE_WITH_KNOTS('',3,(#15078,#15079,#15080,#15081),
 .UNSPECIFIED.,.F.,.F.,(4,4),(0.,1.),.UNSPECIFIED.);
#677=B_SPLINE_CURVE_WITH_KNOTS('',3,(#15084,#15085,#15086,#15087),
 .UNSPECIFIED.,.F.,.F.,(4,4),(4.16666666447352E-8,1.),.UNSPECIFIED.);
#678=B_SPLINE_CURVE_WITH_KNOTS('',3,(#15089,#15090,#15091,#15092),
 .UNSPECIFIED.,.F.,.F.,(4,4),(0.,1.),.UNSPECIFIED.);
#679=B_SPLINE_CURVE_WITH_KNOTS('',3,(#15094,#15095,#15096,#15097),
 .UNSPECIFIED.,.F.,.F.,(4,4),(0.,1.),.UNSPECIFIED.);
#680=B_SPLINE_CURVE_WITH_KNOTS('',3,(#15099,#15100,#15101,#15102),
 .UNSPECIFIED.,.F.,.F.,(4,4),(0.,1.),.UNSPECIFIED.);
#681=B_SPLINE_CURVE_WITH_KNOTS('',3,(#15105,#15106,#15107,#15108),
 .UNSPECIFIED.,.F.,.F.,(4,4),(4.16666666447351E-8,1.),.UNSPECIFIED.);
#682=B_SPLINE_CURVE_WITH_KNOTS('',3,(#15110,#15111,#15112,#15113),
 .UNSPECIFIED.,.F.,.F.,(4,4),(0.,1.),.UNSPECIFIED.);
#683=B_SPLINE_CURVE_WITH_KNOTS('',3,(#15115,#15116,#15117,#15118),
 .UNSPECIFIED.,.F.,.F.,(4,4),(0.,1.),.UNSPECIFIED.);
#684=B_SPLINE_CURVE_WITH_KNOTS('',3,(#15120,#15121,#15122,#15123),
 .UNSPECIFIED.,.F.,.F.,(4,4),(0.,1.),.UNSPECIFIED.);
#685=B_SPLINE_CURVE_WITH_KNOTS('',3,(#15126,#15127,#15128,#15129),
 .UNSPECIFIED.,.F.,.F.,(4,4),(4.16666666447352E-8,1.),.UNSPECIFIED.);
#686=B_SPLINE_CURVE_WITH_KNOTS('',3,(#15131,#15132,#15133,#15134),
 .UNSPECIFIED.,.F.,.F.,(4,4),(0.,1.),.UNSPECIFIED.);
#687=B_SPLINE_CURVE_WITH_KNOTS('',3,(#15136,#15137,#15138,#15139),
 .UNSPECIFIED.,.F.,.F.,(4,4),(0.,1.),.UNSPECIFIED.);
#688=B_SPLINE_CURVE_WITH_KNOTS('',3,(#15141,#15142,#15143,#15144),
 .UNSPECIFIED.,.F.,.F.,(4,4),(0.,1.),.UNSPECIFIED.);
#689=B_SPLINE_CURVE_WITH_KNOTS('',3,(#15150,#15151,#15152,#15153,#15154,
#15155,#15156,#15157,#15158,#15159,#15160),.UNSPECIFIED.,.F.,.F.,(4,1,1,
1,1,1,1,1,4),(1.82133860695804E-10,0.125000000151206,0.250000000120279,
0.375000000089351,0.500000000058424,0.625000000027496,0.749999999996569,
0.874999999965641,0.999999999934714),.UNSPECIFIED.);
#690=B_SPLINE_CURVE_WITH_KNOTS('',3,(#15165,#15166,#15167,#15168,#15169,
#15170,#15171,#15172,#15173,#15174,#15175),.UNSPECIFIED.,.F.,.F.,(4,1,1,
1,1,1,1,1,4),(0.,0.125,0.25,0.375,0.5,0.625,0.75,0.875,1.),
 .UNSPECIFIED.);
#691=B_SPLINE_CURVE_WITH_KNOTS('',3,(#15180,#15181,#15182,#15183,#15184,
#15185,#15186,#15187,#15188,#15189,#15190),.UNSPECIFIED.,.F.,.F.,(4,1,1,
1,1,1,1,1,4),(1.08557388758105E-10,0.125000000084605,0.250000000060653,
0.375000000036701,0.500000000012749,0.624999999988797,0.749999999964844,
0.874999999940892,0.99999999991694),.UNSPECIFIED.);
#692=B_SPLINE_CURVE_WITH_KNOTS('',3,(#15195,#15196,#15197,#15198,#15199,
#15200,#15201,#15202,#15203,#15204,#15205),.UNSPECIFIED.,.F.,.F.,(4,1,1,
1,1,1,1,1,4),(2.37189827595616E-10,0.125000000203968,0.250000000170747,
0.375000000137525,0.500000000104304,0.625000000071082,0.750000000037861,
0.875000000004639,0.999999999971418),.UNSPECIFIED.);
#693=B_SPLINE_CURVE_WITH_KNOTS('',3,(#15214,#15215,#15216,#15217,#15218,
#15219,#15220,#15221,#15222,#15223,#15224),.UNSPECIFIED.,.F.,.F.,(4,1,1,
1,1,1,1,1,4),(0.,0.124999999998599,0.249999999997198,0.374999999995797,
0.499999999994397,0.624999999992996,0.749999999991595,0.874999999990194,
0.999999999988793),.UNSPECIFIED.);
#694=B_SPLINE_CURVE_WITH_KNOTS('',3,(#15229,#15230,#15231,#15232),
 .UNSPECIFIED.,.F.,.F.,(4,4),(0.,1.),.UNSPECIFIED.);
#695=B_SPLINE_CURVE_WITH_KNOTS('',3,(#15236,#15237,#15238,#15239),
 .UNSPECIFIED.,.F.,.F.,(4,4),(0.,1.),.UNSPECIFIED.);
#696=B_SPLINE_CURVE_WITH_KNOTS('',3,(#15243,#15244,#15245,#15246),
 .UNSPECIFIED.,.F.,.F.,(4,4),(0.,0.999999991856635),.UNSPECIFIED.);
#697=B_SPLINE_CURVE_WITH_KNOTS('',3,(#15250,#15251,#15252,#15253),
 .UNSPECIFIED.,.F.,.F.,(4,4),(0.,1.),.UNSPECIFIED.);
#698=B_SPLINE_CURVE_WITH_KNOTS('',3,(#15257,#15258,#15259,#15260),
 .UNSPECIFIED.,.F.,.F.,(4,4),(0.,1.),.UNSPECIFIED.);
#699=B_SPLINE_CURVE_WITH_KNOTS('',3,(#15264,#15265,#15266,#15267),
 .UNSPECIFIED.,.F.,.F.,(4,4),(8.91275946058781E-10,1.),.UNSPECIFIED.);
#700=B_SPLINE_CURVE_WITH_KNOTS('',3,(#15271,#15272,#15273,#15274),
 .UNSPECIFIED.,.F.,.F.,(4,4),(0.,0.999999991166321),.UNSPECIFIED.);
#701=B_SPLINE_CURVE_WITH_KNOTS('',3,(#15278,#15279,#15280,#15281),
 .UNSPECIFIED.,.F.,.F.,(4,4),(0.,1.),.UNSPECIFIED.);
#702=B_SPLINE_CURVE_WITH_KNOTS('',3,(#15285,#15286,#15287,#15288),
 .UNSPECIFIED.,.F.,.F.,(4,4),(0.,0.999999991635845),.UNSPECIFIED.);
#703=B_SPLINE_CURVE_WITH_KNOTS('',3,(#15292,#15293,#15294,#15295),
 .UNSPECIFIED.,.F.,.F.,(4,4),(0.,1.),.UNSPECIFIED.);
#704=B_SPLINE_CURVE_WITH_KNOTS('',3,(#15299,#15300,#15301,#15302),
 .UNSPECIFIED.,.F.,.F.,(4,4),(0.,0.999999990695087),.UNSPECIFIED.);
#705=B_SPLINE_CURVE_WITH_KNOTS('',3,(#15306,#15307,#15308,#15309),
 .UNSPECIFIED.,.F.,.F.,(4,4),(6.70478438173798E-10,1.),.UNSPECIFIED.);
#706=B_SPLINE_CURVE_WITH_KNOTS('',3,(#15329,#15330,#15331,#15332),
 .UNSPECIFIED.,.F.,.F.,(4,4),(0.,1.),.UNSPECIFIED.);
#707=B_SPLINE_CURVE_WITH_KNOTS('',3,(#15334,#15335,#15336,#15337),
 .UNSPECIFIED.,.F.,.F.,(4,4),(3.58215183541293E-10,0.000343052456161631),
 .UNSPECIFIED.);
#708=B_SPLINE_CURVE_WITH_KNOTS('',3,(#15339,#15340,#15341,#15342),
 .UNSPECIFIED.,.F.,.F.,(4,4),(3.65096538768038E-8,0.999999982920268),
 .UNSPECIFIED.);
#709=B_SPLINE_CURVE_WITH_KNOTS('',3,(#15344,#15345,#15346,#15347),
 .UNSPECIFIED.,.F.,.F.,(4,4),(0.,0.000343052524018004),.UNSPECIFIED.);
#710=B_SPLINE_CURVE_WITH_KNOTS('',3,(#15349,#15350,#15351,#15352),
 .UNSPECIFIED.,.F.,.F.,(4,4),(0.,1.),.UNSPECIFIED.);
#711=B_SPLINE_CURVE_WITH_KNOTS('',3,(#15354,#15355,#15356,#15357),
 .UNSPECIFIED.,.F.,.F.,(4,4),(3.26629103003972E-10,0.000343052385686348),
 .UNSPECIFIED.);
#712=B_SPLINE_CURVE_WITH_KNOTS('',3,(#15361,#15362,#15363,#15364),
 .UNSPECIFIED.,.F.,.F.,(4,4),(0.,0.000343052455136989),.UNSPECIFIED.);
#713=B_SPLINE_CURVE_WITH_KNOTS('',3,(#15366,#15367,#15368,#15369),
 .UNSPECIFIED.,.F.,.F.,(4,4),(0.,0.999999999067061),.UNSPECIFIED.);
#714=B_SPLINE_CURVE_WITH_KNOTS('',3,(#15371,#15372,#15373,#15374),
 .UNSPECIFIED.,.F.,.F.,(4,4),(3.60835728632106E-10,0.000343052452422124),
 .UNSPECIFIED.);
#715=B_SPLINE_CURVE_WITH_KNOTS('',3,(#15376,#15377,#15378,#15379),
 .UNSPECIFIED.,.F.,.F.,(4,4),(3.41089703588926E-8,0.999999981759078),
 .UNSPECIFIED.);
#716=B_SPLINE_CURVE_WITH_KNOTS('',3,(#15381,#15382,#15383,#15384),
 .UNSPECIFIED.,.F.,.F.,(4,4),(0.,0.000343052525875007),.UNSPECIFIED.);
#717=B_SPLINE_CURVE_WITH_KNOTS('',3,(#15386,#15387,#15388,#15389),
 .UNSPECIFIED.,.F.,.F.,(4,4),(0.,0.999999997808727),.UNSPECIFIED.);
#718=B_SPLINE_CURVE_WITH_KNOTS('',3,(#15393,#15394,#15395,#15396),
 .UNSPECIFIED.,.F.,.F.,(4,4),(0.,0.000343052525807486),.UNSPECIFIED.);
#719=B_SPLINE_CURVE_WITH_KNOTS('',3,(#15399,#15400,#15401,#15402),
 .UNSPECIFIED.,.F.,.F.,(4,4),(0.,0.999999998658949),.UNSPECIFIED.);
#720=B_SPLINE_CURVE_WITH_KNOTS('',3,(#15403,#15404,#15405,#15406),
 .UNSPECIFIED.,.F.,.F.,(4,4),(0.,0.99999999962777),.UNSPECIFIED.);
#721=B_SPLINE_CURVE_WITH_KNOTS('',3,(#15408,#15409,#15410,#15411),
 .UNSPECIFIED.,.F.,.F.,(4,4),(3.57901911661657E-10,0.000343052455535201),
 .UNSPECIFIED.);
#722=B_SPLINE_CURVE_WITH_KNOTS('',3,(#15413,#15414,#15415,#15416),
 .UNSPECIFIED.,.F.,.F.,(4,4),(3.64646145125801E-8,0.999999982935945),
 .UNSPECIFIED.);
#723=B_SPLINE_CURVE_WITH_KNOTS('',3,(#15418,#15419,#15420,#15421),
 .UNSPECIFIED.,.F.,.F.,(4,4),(0.,0.000343052484606286),.UNSPECIFIED.);
#724=B_SPLINE_CURVE_WITH_KNOTS('',3,(#15423,#15424,#15425,#15426),
 .UNSPECIFIED.,.F.,.F.,(4,4),(0.,0.999999999941115),.UNSPECIFIED.);
#725=B_SPLINE_CURVE_WITH_KNOTS('',3,(#15428,#15429,#15430,#15431),
 .UNSPECIFIED.,.F.,.F.,(4,4),(3.61573077407582E-10,0.000343052449740987),
 .UNSPECIFIED.);
#726=B_SPLINE_CURVE_WITH_KNOTS('',3,(#15433,#15434,#15435,#15436),
 .UNSPECIFIED.,.F.,.F.,(4,4),(3.74094535835276E-8,0.999999981302811),
 .UNSPECIFIED.);
#727=B_SPLINE_CURVE_WITH_KNOTS('',3,(#15438,#15439,#15440,#15441),
 .UNSPECIFIED.,.F.,.F.,(4,4),(0.,0.000343052521102341),.UNSPECIFIED.);
#728=B_SPLINE_CURVE_WITH_KNOTS('',3,(#15443,#15444,#15445,#15446),
 .UNSPECIFIED.,.F.,.F.,(4,4),(0.,0.999999999492176),.UNSPECIFIED.);
#729=B_SPLINE_CURVE_WITH_KNOTS('',3,(#15448,#15449,#15450,#15451),
 .UNSPECIFIED.,.F.,.F.,(4,4),(3.60479596378399E-10,0.000343052451752998),
 .UNSPECIFIED.);
#730=B_SPLINE_CURVE_WITH_KNOTS('',3,(#15453,#15454,#15455,#15456),
 .UNSPECIFIED.,.F.,.F.,(4,4),(3.41403005359674E-8,0.999999981774713),
 .UNSPECIFIED.);
#731=B_SPLINE_CURVE_WITH_KNOTS('',3,(#15461,#15462,#15463,#15464,#15465),
 .UNSPECIFIED.,.F.,.F.,(4,1,4),(0.,0.5,1.),.UNSPECIFIED.);
#732=B_SPLINE_CURVE_WITH_KNOTS('',3,(#15470,#15471,#15472,#15473),
 .UNSPECIFIED.,.F.,.F.,(4,4),(0.,1.),.UNSPECIFIED.);
#733=B_SPLINE_CURVE_WITH_KNOTS('',3,(#15474,#15475,#15476,#15477),
 .UNSPECIFIED.,.F.,.F.,(4,4),(0.,1.),.UNSPECIFIED.);
#734=B_SPLINE_CURVE_WITH_KNOTS('',3,(#15479,#15480,#15481,#15482,#15483,
#15484,#15485),.UNSPECIFIED.,.F.,.F.,(4,1,1,1,4),(-2.56869318007201E-15,
0.249999999983678,0.499999999967359,0.749999999951039,0.99999999993472),
 .UNSPECIFIED.);
#735=B_SPLINE_CURVE_WITH_KNOTS('',3,(#15487,#15488,#15489,#15490),
 .UNSPECIFIED.,.F.,.F.,(4,4),(0.,0.999999999325284),.UNSPECIFIED.);
#736=B_SPLINE_CURVE_WITH_KNOTS('',3,(#15497,#15498,#15499,#15500,#15501),
 .UNSPECIFIED.,.F.,.F.,(4,1,4),(0.,0.5,1.),.UNSPECIFIED.);
#737=B_SPLINE_CURVE_WITH_KNOTS('',3,(#15511,#15512,#15513,#15514),
 .UNSPECIFIED.,.F.,.F.,(4,4),(0.,1.),.UNSPECIFIED.);
#738=B_SPLINE_CURVE_WITH_KNOTS('',3,(#15515,#15516,#15517,#15518),
 .UNSPECIFIED.,.F.,.F.,(4,4),(0.,1.),.UNSPECIFIED.);
#739=B_SPLINE_CURVE_WITH_KNOTS('',3,(#15522,#15523,#15524,#15525,#15526),
 .UNSPECIFIED.,.F.,.F.,(4,1,4),(0.,0.5,1.),.UNSPECIFIED.);
#740=B_SPLINE_CURVE_WITH_KNOTS('',3,(#15531,#15532,#15533,#15534),
 .UNSPECIFIED.,.F.,.F.,(4,4),(2.19687401555071E-9,0.00876797316768544),
 .UNSPECIFIED.);
#741=B_SPLINE_CURVE_WITH_KNOTS('',3,(#15536,#15537,#15538,#15539),
 .UNSPECIFIED.,.F.,.F.,(4,4),(0.,0.999999810914528),.UNSPECIFIED.);
#742=B_SPLINE_CURVE_WITH_KNOTS('',3,(#15541,#15542,#15543,#15544),
 .UNSPECIFIED.,.F.,.F.,(4,4),(1.5598153650561E-11,0.000115526634783486),
 .UNSPECIFIED.);
#743=B_SPLINE_CURVE_WITH_KNOTS('',3,(#15545,#15546,#15547,#15548),
 .UNSPECIFIED.,.F.,.F.,(4,4),(2.45933409031924E-8,1.),.UNSPECIFIED.);
#744=B_SPLINE_CURVE_WITH_KNOTS('',3,(#15550,#15551,#15552,#15553),
 .UNSPECIFIED.,.F.,.F.,(4,4),(0.,0.000461780122359631),.UNSPECIFIED.);
#745=B_SPLINE_CURVE_WITH_KNOTS('',3,(#15555,#15556,#15557,#15558),
 .UNSPECIFIED.,.F.,.F.,(4,4),(1.86650584960977E-10,0.999999999799147),
 .UNSPECIFIED.);
#746=B_SPLINE_CURVE_WITH_KNOTS('',3,(#15560,#15561,#15562,#15563),
 .UNSPECIFIED.,.F.,.F.,(4,4),(-0.000178154369988799,0.000282469411184293),
 .UNSPECIFIED.);
#747=B_SPLINE_CURVE_WITH_KNOTS('',3,(#15565,#15566,#15567,#15568),
 .UNSPECIFIED.,.F.,.F.,(4,4),(0.,0.000115526639299657),.UNSPECIFIED.);
#748=B_SPLINE_CURVE_WITH_KNOTS('',3,(#15570,#15571,#15572,#15573),
 .UNSPECIFIED.,.F.,.F.,(4,4),(3.53200758195611E-7,1.),.UNSPECIFIED.);
#749=B_SPLINE_CURVE_WITH_KNOTS('',3,(#15575,#15576,#15577,#15578),
 .UNSPECIFIED.,.F.,.F.,(4,4),(0.,0.00876797281533553),.UNSPECIFIED.);
#750=B_SPLINE_CURVE_WITH_KNOTS('',3,(#15579,#15580,#15581,#15582),
 .UNSPECIFIED.,.F.,.F.,(4,4),(1.21975118277068E-8,0.999999969283181),
 .UNSPECIFIED.);
#751=B_SPLINE_CURVE_WITH_KNOTS('',3,(#15584,#15585,#15586,#15587),
 .UNSPECIFIED.,.F.,.F.,(4,4),(0.,1.),.UNSPECIFIED.);
#752=B_SPLINE_CURVE_WITH_KNOTS('',3,(#15589,#15590,#15591,#15592),
 .UNSPECIFIED.,.F.,.F.,(4,4),(2.19679543549726E-9,0.00876797316357997),
 .UNSPECIFIED.);
#753=B_SPLINE_CURVE_WITH_KNOTS('',3,(#15594,#15595,#15596,#15597),
 .UNSPECIFIED.,.F.,.F.,(4,4),(0.,0.99999981091663),.UNSPECIFIED.);
#754=B_SPLINE_CURVE_WITH_KNOTS('',3,(#15599,#15600,#15601,#15602),
 .UNSPECIFIED.,.F.,.F.,(4,4),(1.36153440382503E-11,0.000115526633265117),
 .UNSPECIFIED.);
#755=B_SPLINE_CURVE_WITH_KNOTS('',3,(#15604,#15605,#15606,#15607),
 .UNSPECIFIED.,.F.,.F.,(4,4),(0.,0.000461390340959227),.UNSPECIFIED.);
#756=B_SPLINE_CURVE_WITH_KNOTS('',3,(#15609,#15610,#15611,#15612),
 .UNSPECIFIED.,.F.,.F.,(4,4),(6.51238540302813E-9,0.999999991006167),
 .UNSPECIFIED.);
#757=B_SPLINE_CURVE_WITH_KNOTS('',3,(#15614,#15615,#15616,#15617),
 .UNSPECIFIED.,.F.,.F.,(4,4),(4.44834970861248E-11,0.000461780122269224),
 .UNSPECIFIED.);
#758=B_SPLINE_CURVE_WITH_KNOTS('',3,(#15619,#15620,#15621,#15622),
 .UNSPECIFIED.,.F.,.F.,(4,4),(0.,0.000115526639624777),.UNSPECIFIED.);
#759=B_SPLINE_CURVE_WITH_KNOTS('',3,(#15624,#15625,#15626,#15627),
 .UNSPECIFIED.,.F.,.F.,(4,4),(3.53210884617722E-7,1.),.UNSPECIFIED.);
#760=B_SPLINE_CURVE_WITH_KNOTS('',3,(#15629,#15630,#15631,#15632),
 .UNSPECIFIED.,.F.,.F.,(4,4),(0.,0.00876797281938125),.UNSPECIFIED.);
#761=B_SPLINE_CURVE_WITH_KNOTS('',3,(#15633,#15634,#15635,#15636),
 .UNSPECIFIED.,.F.,.F.,(4,4),(0.,0.999999969357093),.UNSPECIFIED.);
#762=B_SPLINE_CURVE_WITH_KNOTS('',3,(#15638,#15639,#15640,#15641),
 .UNSPECIFIED.,.F.,.F.,(4,4),(0.,1.),.UNSPECIFIED.);
#763=B_SPLINE_CURVE_WITH_KNOTS('',3,(#15643,#15644,#15645,#15646),
 .UNSPECIFIED.,.F.,.F.,(4,4),(7.85920675138078E-11,0.000507167122736054),
 .UNSPECIFIED.);
#764=B_SPLINE_CURVE_WITH_KNOTS('',3,(#15648,#15649,#15650,#15651),
 .UNSPECIFIED.,.F.,.F.,(4,4),(0.,1.),.UNSPECIFIED.);
#765=B_SPLINE_CURVE_WITH_KNOTS('',3,(#15659,#15660,#15661,#15662),
 .UNSPECIFIED.,.F.,.F.,(4,4),(4.44935875990053E-11,0.000461780122658492),
 .UNSPECIFIED.);
#766=B_SPLINE_CURVE_WITH_KNOTS('',3,(#15664,#15665,#15666,#15667),
 .UNSPECIFIED.,.F.,.F.,(4,4),(0.,0.000115526643526207),.UNSPECIFIED.);
#767=B_SPLINE_CURVE_WITH_KNOTS('',3,(#15669,#15670,#15671,#15672),
 .UNSPECIFIED.,.F.,.F.,(4,4),(1.21975111506088E-8,0.999999969326361),
 .UNSPECIFIED.);
#768=B_SPLINE_CURVE_WITH_KNOTS('',3,(#15673,#15674,#15675,#15676),
 .UNSPECIFIED.,.F.,.F.,(4,4),(3.53216997744741E-7,1.),.UNSPECIFIED.);
#769=B_SPLINE_CURVE_WITH_KNOTS('',3,(#15678,#15679,#15680,#15681),
 .UNSPECIFIED.,.F.,.F.,(4,4),(0.,0.00876797288604423),.UNSPECIFIED.);
#770=B_SPLINE_CURVE_WITH_KNOTS('',3,(#15683,#15684,#15685,#15686),
 .UNSPECIFIED.,.F.,.F.,(4,4),(0.,1.),.UNSPECIFIED.);
#771=B_SPLINE_CURVE_WITH_KNOTS('',3,(#15688,#15689,#15690,#15691),
 .UNSPECIFIED.,.F.,.F.,(4,4),(2.19806870576548E-9,0.00876797316802286),
 .UNSPECIFIED.);
#772=B_SPLINE_CURVE_WITH_KNOTS('',3,(#15693,#15694,#15695,#15696),
 .UNSPECIFIED.,.F.,.F.,(4,4),(0.,0.999999810910841),.UNSPECIFIED.);
#773=B_SPLINE_CURVE_WITH_KNOTS('',3,(#15698,#15699,#15700,#15701),
 .UNSPECIFIED.,.F.,.F.,(4,4),(1.55981466010636E-11,0.000115526634759396),
 .UNSPECIFIED.);
#774=B_SPLINE_CURVE_WITH_KNOTS('',3,(#15703,#15704,#15705,#15706),
 .UNSPECIFIED.,.F.,.F.,(4,4),(0.,0.000461780122378384),.UNSPECIFIED.);
#775=B_SPLINE_CURVE_WITH_KNOTS('',3,(#15708,#15709,#15710,#15711),
 .UNSPECIFIED.,.F.,.F.,(4,4),(2.06223918325493E-10,0.999999990931219),
 .UNSPECIFIED.);
#776=B_SPLINE_CURVE_WITH_KNOTS('',3,(#15713,#15714,#15715,#15716),
 .UNSPECIFIED.,.F.,.F.,(4,4),(4.45944620771068E-11,0.000461780122150718),
 .UNSPECIFIED.);
#777=B_SPLINE_CURVE_WITH_KNOTS('',3,(#15718,#15719,#15720,#15721),
 .UNSPECIFIED.,.F.,.F.,(4,4),(0.,0.000115526634772737),.UNSPECIFIED.);
#778=B_SPLINE_CURVE_WITH_KNOTS('',3,(#15723,#15724,#15725,#15726),
 .UNSPECIFIED.,.F.,.F.,(4,4),(3.53260322116059E-7,1.),.UNSPECIFIED.);
#779=B_SPLINE_CURVE_WITH_KNOTS('',3,(#15728,#15729,#15730,#15731),
 .UNSPECIFIED.,.F.,.F.,(4,4),(0.,0.0087679728154019),.UNSPECIFIED.);
#780=B_SPLINE_CURVE_WITH_KNOTS('',3,(#15732,#15733,#15734,#15735),
 .UNSPECIFIED.,.F.,.F.,(4,4),(1.21975118277068E-8,0.999999969283181),
 .UNSPECIFIED.);
#781=B_SPLINE_CURVE_WITH_KNOTS('',3,(#15737,#15738,#15739,#15740),
 .UNSPECIFIED.,.F.,.F.,(4,4),(0.,1.),.UNSPECIFIED.);
#782=B_SPLINE_CURVE_WITH_KNOTS('',3,(#15742,#15743,#15744,#15745),
 .UNSPECIFIED.,.F.,.F.,(4,4),(2.19700664975534E-9,0.00876797316368185),
 .UNSPECIFIED.);
#783=B_SPLINE_CURVE_WITH_KNOTS('',3,(#15747,#15748,#15749,#15750),
 .UNSPECIFIED.,.F.,.F.,(4,4),(0.,0.999999810875566),.UNSPECIFIED.);
#784=B_SPLINE_CURVE_WITH_KNOTS('',3,(#15752,#15753,#15754,#15755),
 .UNSPECIFIED.,.F.,.F.,(4,4),(1.36153488748495E-11,0.000115526628722257),
 .UNSPECIFIED.);
#785=B_SPLINE_CURVE_WITH_KNOTS('',3,(#15757,#15758,#15759,#15760),
 .UNSPECIFIED.,.F.,.F.,(4,4),(0.,0.000461780122286861),.UNSPECIFIED.);
#786=B_SPLINE_CURVE_WITH_KNOTS('',3,(#15762,#15763,#15764,#15765),
 .UNSPECIFIED.,.F.,.F.,(4,4),(2.36216418598326E-10,0.999999991023223),
 .UNSPECIFIED.);
#787=B_SPLINE_CURVE_WITH_KNOTS('',3,(#15767,#15768,#15769,#15770),
 .UNSPECIFIED.,.F.,.F.,(4,4),(4.44686267605015E-11,0.000461780122242359),
 .UNSPECIFIED.);
#788=B_SPLINE_CURVE_WITH_KNOTS('',3,(#15772,#15773,#15774,#15775),
 .UNSPECIFIED.,.F.,.F.,(4,4),(0.,0.000115526639658502),.UNSPECIFIED.);
#789=B_SPLINE_CURVE_WITH_KNOTS('',3,(#15777,#15778,#15779,#15780),
 .UNSPECIFIED.,.F.,.F.,(4,4),(3.53305356218227E-7,1.),.UNSPECIFIED.);
#790=B_SPLINE_CURVE_WITH_KNOTS('',3,(#15782,#15783,#15784,#15785),
 .UNSPECIFIED.,.F.,.F.,(4,4),(0.,0.0087679728211208),.UNSPECIFIED.);
#791=B_SPLINE_CURVE_WITH_KNOTS('',3,(#15786,#15787,#15788,#15789),
 .UNSPECIFIED.,.F.,.F.,(4,4),(1.21975111506088E-8,0.999999969357093),
 .UNSPECIFIED.);
#792=B_SPLINE_CURVE_WITH_KNOTS('',3,(#15791,#15792,#15793,#15794),
 .UNSPECIFIED.,.F.,.F.,(4,4),(0.,1.),.UNSPECIFIED.);
#793=B_SPLINE_CURVE_WITH_KNOTS('',3,(#15796,#15797,#15798,#15799),
 .UNSPECIFIED.,.F.,.F.,(4,4),(2.19702460833624E-9,0.00876797316930945),
 .UNSPECIFIED.);
#794=B_SPLINE_CURVE_WITH_KNOTS('',3,(#15801,#15802,#15803,#15804),
 .UNSPECIFIED.,.F.,.F.,(4,4),(0.,0.999999810901908),.UNSPECIFIED.);
#795=B_SPLINE_CURVE_WITH_KNOTS('',3,(#15806,#15807,#15808,#15809),
 .UNSPECIFIED.,.F.,.F.,(4,4),(1.79267076322998E-11,0.00011552663817591),
 .UNSPECIFIED.);
#796=B_SPLINE_CURVE_WITH_KNOTS('',3,(#15811,#15812,#15813,#15814),
 .UNSPECIFIED.,.F.,.F.,(4,4),(0.,0.000461780123066742),.UNSPECIFIED.);
#797=B_SPLINE_CURVE_WITH_KNOTS('',3,(#15816,#15817,#15818,#15819),
 .UNSPECIFIED.,.F.,.F.,(4,4),(2.5020233577996E-10,0.99999999095112),
 .UNSPECIFIED.);
#798=B_SPLINE_CURVE_WITH_KNOTS('',3,(#15821,#15822,#15823,#15824),
 .UNSPECIFIED.,.F.,.F.,(4,4),(4.44328322544207E-11,0.000461780122903715),
 .UNSPECIFIED.);
#799=B_SPLINE_CURVE_WITH_KNOTS('',3,(#15826,#15827,#15828,#15829),
 .UNSPECIFIED.,.F.,.F.,(4,4),(0.,0.000115526643559045),.UNSPECIFIED.);
#800=B_SPLINE_CURVE_WITH_KNOTS('',3,(#15831,#15832,#15833,#15834),
 .UNSPECIFIED.,.F.,.F.,(4,4),(3.53157909585551E-7,1.),.UNSPECIFIED.);
#801=B_SPLINE_CURVE_WITH_KNOTS('',3,(#15836,#15837,#15838,#15839),
 .UNSPECIFIED.,.F.,.F.,(4,4),(0.,0.00876797282088719),.UNSPECIFIED.);
#802=B_SPLINE_CURVE_WITH_KNOTS('',3,(#15840,#15841,#15842,#15843),
 .UNSPECIFIED.,.F.,.F.,(4,4),(1.21975111506088E-8,0.999999969326361),
 .UNSPECIFIED.);
#803=B_SPLINE_CURVE_WITH_KNOTS('',3,(#15846,#15847,#15848,#15849),
 .UNSPECIFIED.,.F.,.F.,(4,4),(0.,5.47511884554027E-5),.UNSPECIFIED.);
#804=B_SPLINE_CURVE_WITH_KNOTS('',3,(#15851,#15852,#15853,#15854),
 .UNSPECIFIED.,.F.,.F.,(4,4),(0.,1.),.UNSPECIFIED.);
#805=B_SPLINE_CURVE_WITH_KNOTS('',3,(#15856,#15857,#15858,#15859),
 .UNSPECIFIED.,.F.,.F.,(4,4),(2.6662045205095E-15,5.47511885493758E-5),
 .UNSPECIFIED.);
#806=B_SPLINE_CURVE_WITH_KNOTS('',3,(#15860,#15861,#15862,#15863,#15864,
#15865,#15866,#15867,#15868),.UNSPECIFIED.,.F.,.F.,(4,1,1,1,1,1,4),(0.,
0.25,0.375,0.5,0.625,0.75,1.),.UNSPECIFIED.);
#807=B_SPLINE_CURVE_WITH_KNOTS('',3,(#15871,#15872,#15873,#15874,#15875,
#15876,#15877,#15878,#15879,#15880),.UNSPECIFIED.,.F.,.F.,(4,1,1,1,1,1,
1,4),(0.,0.25,0.375,0.5,0.625,0.75,0.875,1.),.UNSPECIFIED.);
#808=B_SPLINE_CURVE_WITH_KNOTS('',3,(#15882,#15883,#15884,#15885),
 .UNSPECIFIED.,.F.,.F.,(4,4),(0.,5.47504762023892E-5),.UNSPECIFIED.);
#809=B_SPLINE_CURVE_WITH_KNOTS('',3,(#15889,#15890,#15891,#15892),
 .UNSPECIFIED.,.F.,.F.,(4,4),(5.41713412566433E-5,0.999997965428435),
 .UNSPECIFIED.);
#810=B_SPLINE_CURVE_WITH_KNOTS('',3,(#15894,#15895,#15896,#15897),
 .UNSPECIFIED.,.F.,.F.,(4,4),(4.31187151013716E-9,0.00876797323705365),
 .UNSPECIFIED.);
#811=B_SPLINE_CURVE_WITH_KNOTS('',3,(#15898,#15899,#15900,#15901,#15902,
#15903,#15904,#15905,#15906),.UNSPECIFIED.,.F.,.F.,(4,1,1,1,1,1,4),(0.,
0.25,0.375,0.5,0.625,0.75,1.),.UNSPECIFIED.);
#812=B_SPLINE_CURVE_WITH_KNOTS('',3,(#15909,#15910,#15911,#15912,#15913,
#15914,#15915,#15916,#15917,#15918),.UNSPECIFIED.,.F.,.F.,(4,1,1,1,1,1,
1,4),(0.,0.25,0.375,0.5,0.625,0.75,0.875,1.),.UNSPECIFIED.);
#813=B_SPLINE_CURVE_WITH_KNOTS('',3,(#15920,#15921,#15922,#15923),
 .UNSPECIFIED.,.F.,.F.,(4,4),(0.,0.999999976739494),.UNSPECIFIED.);
#814=B_SPLINE_CURVE_WITH_KNOTS('',3,(#15925,#15926,#15927,#15928),
 .UNSPECIFIED.,.F.,.F.,(4,4),(0.,5.47511871644386E-5),.UNSPECIFIED.);
#815=B_SPLINE_CURVE_WITH_KNOTS('',3,(#15930,#15931,#15932,#15933),
 .UNSPECIFIED.,.F.,.F.,(4,4),(0.,1.),.UNSPECIFIED.);
#816=B_SPLINE_CURVE_WITH_KNOTS('',3,(#15935,#15936,#15937,#15938),
 .UNSPECIFIED.,.F.,.F.,(4,4),(0.,5.47485615078587E-5),.UNSPECIFIED.);
#817=B_SPLINE_CURVE_WITH_KNOTS('',3,(#15939,#15940,#15941,#15942,#15943,
#15944,#15945,#15946,#15947),.UNSPECIFIED.,.F.,.F.,(4,1,1,1,1,1,4),(0.,
0.25,0.375,0.5,0.625,0.75,1.),.UNSPECIFIED.);
#818=B_SPLINE_CURVE_WITH_KNOTS('',3,(#15950,#15951,#15952,#15953,#15954,
#15955,#15956,#15957,#15958,#15959),.UNSPECIFIED.,.F.,.F.,(4,1,1,1,1,1,
1,4),(0.,0.25,0.375,0.5,0.625,0.75,0.875,1.),.UNSPECIFIED.);
#819=B_SPLINE_CURVE_WITH_KNOTS('',3,(#15961,#15962,#15963,#15964),
 .UNSPECIFIED.,.F.,.F.,(4,4),(0.,5.47504681501983E-5),.UNSPECIFIED.);
#820=B_SPLINE_CURVE_WITH_KNOTS('',3,(#15966,#15967,#15968,#15969),
 .UNSPECIFIED.,.F.,.F.,(4,4),(0.,1.),.UNSPECIFIED.);
#821=B_SPLINE_CURVE_WITH_KNOTS('',3,(#15971,#15972,#15973,#15974),
 .UNSPECIFIED.,.F.,.F.,(4,4),(1.73372280702655E-14,5.47511861723444E-5),
 .UNSPECIFIED.);
#822=B_SPLINE_CURVE_WITH_KNOTS('',3,(#15975,#15976,#15977,#15978,#15979,
#15980,#15981,#15982,#15983),.UNSPECIFIED.,.F.,.F.,(4,1,1,1,1,1,4),(0.,
0.25,0.375,0.5,0.625,0.75,1.),.UNSPECIFIED.);
#823=B_SPLINE_CURVE_WITH_KNOTS('',3,(#15986,#15987,#15988,#15989,#15990,
#15991,#15992,#15993,#15994,#15995),.UNSPECIFIED.,.F.,.F.,(4,1,1,1,1,1,
1,4),(0.,0.25,0.375,0.5,0.625,0.75,0.875,1.),.UNSPECIFIED.);
#824=B_SPLINE_CURVE_WITH_KNOTS('',3,(#15997,#15998,#15999,#16000),
 .UNSPECIFIED.,.F.,.F.,(4,4),(0.,5.4751186768266E-5),.UNSPECIFIED.);
#825=B_SPLINE_CURVE_WITH_KNOTS('',3,(#16002,#16003,#16004,#16005),
 .UNSPECIFIED.,.F.,.F.,(4,4),(0.,1.),.UNSPECIFIED.);
#826=B_SPLINE_CURVE_WITH_KNOTS('',3,(#16007,#16008,#16009,#16010),
 .UNSPECIFIED.,.F.,.F.,(4,4),(2.81166365578815E-14,5.47511864643206E-5),
 .UNSPECIFIED.);
#827=B_SPLINE_CURVE_WITH_KNOTS('',3,(#16011,#16012,#16013,#16014,#16015,
#16016,#16017,#16018,#16019),.UNSPECIFIED.,.F.,.F.,(4,1,1,1,1,1,4),(0.,
0.25,0.375,0.5,0.625,0.75,1.),.UNSPECIFIED.);
#828=B_SPLINE_CURVE_WITH_KNOTS('',3,(#16022,#16023,#16024,#16025,#16026,
#16027,#16028,#16029,#16030,#16031),.UNSPECIFIED.,.F.,.F.,(4,1,1,1,1,1,
1,4),(0.,0.25,0.375,0.5,0.625,0.75,0.875,1.),.UNSPECIFIED.);
#829=B_SPLINE_CURVE_WITH_KNOTS('',3,(#16033,#16034,#16035,#16036),
 .UNSPECIFIED.,.F.,.F.,(4,4),(0.,5.47511848914998E-5),.UNSPECIFIED.);
#830=B_SPLINE_CURVE_WITH_KNOTS('',3,(#16038,#16039,#16040,#16041),
 .UNSPECIFIED.,.F.,.F.,(4,4),(0.,1.),.UNSPECIFIED.);
#831=B_SPLINE_CURVE_WITH_KNOTS('',3,(#16043,#16044,#16045,#16046),
 .UNSPECIFIED.,.F.,.F.,(4,4),(3.54203178136851E-15,5.47511866309463E-5),
 .UNSPECIFIED.);
#832=B_SPLINE_CURVE_WITH_KNOTS('',3,(#16047,#16048,#16049,#16050,#16051,
#16052,#16053,#16054,#16055),.UNSPECIFIED.,.F.,.F.,(4,1,1,1,1,1,4),(0.,
0.25,0.375,0.5,0.625,0.75,1.),.UNSPECIFIED.);
#833=B_SPLINE_CURVE_WITH_KNOTS('',3,(#16058,#16059,#16060,#16061,#16062,
#16063,#16064,#16065,#16066,#16067),.UNSPECIFIED.,.F.,.F.,(4,1,1,1,1,1,
1,4),(0.,0.25,0.375,0.5,0.625,0.75,0.875,1.),.UNSPECIFIED.);
#834=B_SPLINE_CURVE_WITH_KNOTS('',3,(#16069,#16070,#16071,#16072),
 .UNSPECIFIED.,.F.,.F.,(4,4),(0.,0.999999786485093),.UNSPECIFIED.);
#835=B_SPLINE_CURVE_WITH_KNOTS('',3,(#16075,#16076,#16077,#16078,#16079,
#16080,#16081,#16082,#16083,#16084,#16085,#16086,#16087,#16088,#16089,#16090,
#16091,#16092,#16093,#16094,#16095,#16096,#16097,#16098,#16099),
 .UNSPECIFIED.,.F.,.F.,(4,1,1,1,1,1,1,1,1,1,1,1,1,1,1,1,1,1,1,1,1,1,4),
(0.,0.03125,0.046875,0.0625,0.09375,0.125,0.15625,0.1875,0.21875,0.25,0.3125,
0.375,0.4375,0.5,0.625,0.6875,0.75,0.8125,0.875,0.90625,0.9375,0.96875,
1.),.UNSPECIFIED.);
#836=B_SPLINE_CURVE_WITH_KNOTS('',3,(#16101,#16102,#16103,#16104),
 .UNSPECIFIED.,.F.,.F.,(4,4),(0.,1.),.UNSPECIFIED.);
#837=B_SPLINE_CURVE_WITH_KNOTS('',3,(#16106,#16107,#16108,#16109,#16110,
#16111,#16112,#16113,#16114,#16115,#16116,#16117,#16118,#16119,#16120,#16121,
#16122,#16123,#16124),.UNSPECIFIED.,.F.,.F.,(4,1,1,1,1,1,1,1,1,1,1,1,1,
1,1,1,4),(1.7738102471483E-8,0.0625000166294711,0.0937500160751554,0.12500001552084,
0.187500014412208,0.250000013303577,0.312500012194945,0.375000011086314,
0.437500009977683,0.500000008869051,0.625000006651788,0.687500005543157,
0.750000004434526,0.812500003325894,0.875000002217263,0.937500001108631,
1.),.UNSPECIFIED.);
#838=B_SPLINE_CURVE_WITH_KNOTS('',3,(#16126,#16127,#16128,#16129),
 .UNSPECIFIED.,.F.,.F.,(4,4),(0.,0.999999711518337),.UNSPECIFIED.);
#839=B_SPLINE_CURVE_WITH_KNOTS('',3,(#16132,#16133,#16134,#16135,#16136,
#16137,#16138,#16139,#16140,#16141,#16142,#16143,#16144,#16145,#16146,#16147,
#16148,#16149,#16150,#16151,#16152,#16153,#16154,#16155,#16156),
 .UNSPECIFIED.,.F.,.F.,(4,1,1,1,1,1,1,1,1,1,1,1,1,1,1,1,1,1,1,1,1,1,4),
(0.,0.03125,0.046875,0.0625,0.09375,0.125,0.15625,0.1875,0.21875,0.25,0.3125,
0.375,0.4375,0.5,0.625,0.6875,0.75,0.8125,0.875,0.90625,0.9375,0.96875,
1.),.UNSPECIFIED.);
#840=B_SPLINE_CURVE_WITH_KNOTS('',3,(#16158,#16159,#16160,#16161),
 .UNSPECIFIED.,.F.,.F.,(4,4),(0.,1.),.UNSPECIFIED.);
#841=B_SPLINE_CURVE_WITH_KNOTS('',3,(#16163,#16164,#16165,#16166,#16167,
#16168,#16169,#16170,#16171,#16172,#16173,#16174,#16175,#16176,#16177,#16178,
#16179,#16180,#16181),.UNSPECIFIED.,.F.,.F.,(4,1,1,1,1,1,1,1,1,1,1,1,1,
1,1,1,4),(1.77381032905796E-8,0.0625000166294718,0.0937500160751561,0.12500001552084,
0.187500014412209,0.250000013303577,0.312500012194946,0.375000011086315,
0.437500009977683,0.500000008869052,0.625000006651789,0.687500005543157,
0.750000004434526,0.812500003325894,0.875000002217263,0.937500001108631,
1.),.UNSPECIFIED.);
#842=B_SPLINE_CURVE_WITH_KNOTS('',3,(#16183,#16184,#16185,#16186,#16187,
#16188,#16189,#16190,#16191,#16192,#16193,#16194,#16195,#16196,#16197,#16198,
#16199,#16200,#16201,#16202,#16203,#16204,#16205,#16206,#16207),
 .UNSPECIFIED.,.F.,.F.,(4,1,1,1,1,1,1,1,1,1,1,1,1,1,1,1,1,1,1,1,1,1,4),
(0.,0.03125,0.046875,0.0625,0.09375,0.125,0.15625,0.1875,0.21875,0.25,0.3125,
0.375,0.4375,0.5,0.625,0.6875,0.75,0.8125,0.875,0.90625,0.9375,0.96875,
1.),.UNSPECIFIED.);
#843=B_SPLINE_CURVE_WITH_KNOTS('',3,(#16210,#16211,#16212,#16213),
 .UNSPECIFIED.,.F.,.F.,(4,4),(0.,1.),.UNSPECIFIED.);
#844=B_SPLINE_CURVE_WITH_KNOTS('',3,(#16215,#16216,#16217,#16218,#16219,
#16220,#16221,#16222,#16223,#16224,#16225,#16226,#16227,#16228,#16229,#16230,
#16231),.UNSPECIFIED.,.F.,.F.,(4,1,1,1,1,1,1,1,1,1,1,1,1,1,4),(1.7738103310695E-8,
0.0625000166294719,0.0937500160751561,0.12500001552084,0.187500014412209,
0.250000013303577,0.312500012194946,0.375000011086315,0.437500009977683,
0.500000008869052,0.625000006651789,0.750000004434526,0.812500003325894,
0.875000002217263,1.),.UNSPECIFIED.);
#845=B_SPLINE_CURVE_WITH_KNOTS('',3,(#16233,#16234,#16235,#16236),
 .UNSPECIFIED.,.F.,.F.,(4,4),(0.,0.999999786485099),.UNSPECIFIED.);
#846=B_SPLINE_CURVE_WITH_KNOTS('',3,(#16238,#16239,#16240,#16241,#16242,
#16243,#16244,#16245,#16246,#16247,#16248,#16249,#16250,#16251,#16252,#16253,
#16254,#16255,#16256,#16257,#16258,#16259,#16260,#16261,#16262),
 .UNSPECIFIED.,.F.,.F.,(4,1,1,1,1,1,1,1,1,1,1,1,1,1,1,1,1,1,1,1,1,1,4),
(0.,0.03125,0.046875,0.0625,0.09375,0.125,0.15625,0.1875,0.21875,0.25,0.3125,
0.375,0.4375,0.5,0.625,0.6875,0.75,0.8125,0.875,0.90625,0.9375,0.96875,
1.),.UNSPECIFIED.);
#847=B_SPLINE_CURVE_WITH_KNOTS('',3,(#16265,#16266,#16267,#16268),
 .UNSPECIFIED.,.F.,.F.,(4,4),(0.,1.),.UNSPECIFIED.);
#848=B_SPLINE_CURVE_WITH_KNOTS('',3,(#16270,#16271,#16272,#16273,#16274,
#16275,#16276,#16277,#16278,#16279,#16280,#16281,#16282,#16283,#16284,#16285,
#16286,#16287,#16288),.UNSPECIFIED.,.F.,.F.,(4,1,1,1,1,1,1,1,1,1,1,1,1,
1,1,1,4),(1.77381030488726E-8,0.0625000166294716,0.0937500160751559,0.12500001552084,
0.187500014412209,0.250000013303577,0.312500012194946,0.375000011086314,
0.437500009977683,0.500000008869051,0.625000006651789,0.687500005543157,
0.750000004434526,0.812500003325894,0.875000002217263,0.937500001108631,
1.),.UNSPECIFIED.);
#849=B_SPLINE_CURVE_WITH_KNOTS('',3,(#16290,#16291,#16292,#16293),
 .UNSPECIFIED.,.F.,.F.,(4,4),(0.,0.999999786485093),.UNSPECIFIED.);
#850=B_SPLINE_CURVE_WITH_KNOTS('',3,(#16295,#16296,#16297,#16298,#16299,
#16300,#16301,#16302,#16303,#16304,#16305,#16306,#16307,#16308,#16309,#16310,
#16311,#16312,#16313,#16314,#16315,#16316,#16317,#16318,#16319),
 .UNSPECIFIED.,.F.,.F.,(4,1,1,1,1,1,1,1,1,1,1,1,1,1,1,1,1,1,1,1,1,1,4),
(0.,0.03125,0.046875,0.0625,0.09375,0.125,0.15625,0.1875,0.21875,0.25,0.3125,
0.375,0.4375,0.5,0.625,0.6875,0.75,0.8125,0.875,0.90625,0.9375,0.96875,
1.),.UNSPECIFIED.);
#851=B_SPLINE_CURVE_WITH_KNOTS('',3,(#16322,#16323,#16324,#16325),
 .UNSPECIFIED.,.F.,.F.,(4,4),(0.,1.),.UNSPECIFIED.);
#852=B_SPLINE_CURVE_WITH_KNOTS('',3,(#16327,#16328,#16329,#16330,#16331,
#16332,#16333,#16334,#16335,#16336,#16337,#16338,#16339,#16340,#16341,#16342,
#16343,#16344,#16345),.UNSPECIFIED.,.F.,.F.,(4,1,1,1,1,1,1,1,1,1,1,1,1,
1,1,1,4),(2.39185157367047E-8,0.0625000224236085,0.0937500216761549,0.125000020928701,
0.187500019433794,0.250000017938887,0.31250001644398,0.375000014949072,
0.437500013454165,0.500000011959258,0.625000008969443,0.687500007474536,
0.750000005979629,0.812500004484722,0.875000002989815,0.937500001494907,
1.),.UNSPECIFIED.);
#853=B_SPLINE_CURVE_WITH_KNOTS('',3,(#16347,#16348,#16349,#16350),
 .UNSPECIFIED.,.F.,.F.,(4,4),(0.,0.999999786485096),.UNSPECIFIED.);
#854=B_SPLINE_CURVE_WITH_KNOTS('',3,(#16352,#16353,#16354,#16355),
 .UNSPECIFIED.,.F.,.F.,(4,4),(0.,0.999999786485099),.UNSPECIFIED.);
#855=B_SPLINE_CURVE_WITH_KNOTS('',3,(#16358,#16359,#16360,#16361,#16362,
#16363,#16364,#16365,#16366,#16367,#16368,#16369,#16370,#16371,#16372,#16373,
#16374,#16375,#16376,#16377,#16378,#16379,#16380),.UNSPECIFIED.,.F.,.F.,
(4,1,1,1,1,1,1,1,1,1,1,1,1,1,1,1,1,1,1,1,4),(0.,0.03125,0.046875,0.0625,
0.09375,0.125,0.15625,0.1875,0.21875,0.25,0.3125,0.375,0.4375,0.5,0.625,
0.6875,0.75,0.8125,0.875,0.9375,1.),.UNSPECIFIED.);
#856=B_SPLINE_CURVE_WITH_KNOTS('',3,(#16382,#16383,#16384,#16385),
 .UNSPECIFIED.,.F.,.F.,(4,4),(0.,1.),.UNSPECIFIED.);
#857=B_SPLINE_CURVE_WITH_KNOTS('',3,(#16387,#16388,#16389,#16390,#16391,
#16392,#16393,#16394,#16395,#16396,#16397,#16398,#16399,#16400,#16401,#16402,
#16403,#16404,#16405),.UNSPECIFIED.,.F.,.F.,(4,1,1,1,1,1,1,1,1,1,1,1,1,
1,1,1,4),(1.77381032197E-8,0.0625000166294718,0.093750016075156,0.12500001552084,
0.187500014412209,0.250000013303577,0.312500012194946,0.375000011086315,
0.437500009977683,0.500000008869052,0.625000006651789,0.687500005543157,
0.750000004434526,0.812500003325894,0.875000002217263,0.937500001108631,
1.),.UNSPECIFIED.);
#858=B_SPLINE_CURVE_WITH_KNOTS('',3,(#16407,#16408,#16409,#16410),
 .UNSPECIFIED.,.F.,.F.,(4,4),(9.76476175762548E-14,0.000408584948842628),
 .UNSPECIFIED.);
#859=B_SPLINE_CURVE_WITH_KNOTS('',3,(#16412,#16413,#16414,#16415),
 .UNSPECIFIED.,.F.,.F.,(4,4),(0.,1.),.UNSPECIFIED.);
#860=B_SPLINE_CURVE_WITH_KNOTS('',3,(#16417,#16418,#16419,#16420),
 .UNSPECIFIED.,.F.,.F.,(4,4),(0.,0.999999971246998),.UNSPECIFIED.);
#861=B_SPLINE_CURVE_WITH_KNOTS('',3,(#16422,#16423,#16424,#16425),
 .UNSPECIFIED.,.F.,.F.,(4,4),(-0.000178154180456897,0.000230031247706017),
 .UNSPECIFIED.);
#862=B_SPLINE_CURVE_WITH_KNOTS('',3,(#16427,#16428,#16429,#16430),
 .UNSPECIFIED.,.F.,.F.,(4,4),(5.83500099566355E-9,0.999999999974686),
 .UNSPECIFIED.);
#863=B_SPLINE_CURVE_WITH_KNOTS('',3,(#16432,#16433,#16434,#16435),
 .UNSPECIFIED.,.F.,.F.,(4,4),(8.66730814626801E-10,0.00040832854943033),
 .UNSPECIFIED.);
#864=B_SPLINE_CURVE_WITH_KNOTS('',3,(#16437,#16438,#16439,#16440),
 .UNSPECIFIED.,.F.,.F.,(4,4),(0.,1.),.UNSPECIFIED.);
#865=B_SPLINE_CURVE_WITH_KNOTS('',3,(#16442,#16443,#16444,#16445),
 .UNSPECIFIED.,.F.,.F.,(4,4),(8.74189910716064E-10,0.000408584947659101),
 .UNSPECIFIED.);
#866=B_SPLINE_CURVE_WITH_KNOTS('',3,(#16447,#16448,#16449,#16450),
 .UNSPECIFIED.,.F.,.F.,(4,4),(0.,1.),.UNSPECIFIED.);
#867=B_SPLINE_CURVE_WITH_KNOTS('',3,(#16452,#16453,#16454,#16455),
 .UNSPECIFIED.,.F.,.F.,(4,4),(0.,1.),.UNSPECIFIED.);
#868=B_SPLINE_CURVE_WITH_KNOTS('',3,(#16457,#16458,#16459,#16460),
 .UNSPECIFIED.,.F.,.F.,(4,4),(1.74701212203631E-8,1.),.UNSPECIFIED.);
#869=B_SPLINE_CURVE_WITH_KNOTS('',3,(#16462,#16463,#16464,#16465),
 .UNSPECIFIED.,.F.,.F.,(4,4),(0.,1.),.UNSPECIFIED.);
#870=B_SPLINE_CURVE_WITH_KNOTS('',3,(#16467,#16468,#16469,#16470),
 .UNSPECIFIED.,.F.,.F.,(4,4),(1.22431959981855E-9,0.000408585660822127),
 .UNSPECIFIED.);
#871=B_SPLINE_CURVE_WITH_KNOTS('',3,(#16472,#16473,#16474,#16475),
 .UNSPECIFIED.,.F.,.F.,(4,4),(0.,1.),.UNSPECIFIED.);
#872=B_SPLINE_CURVE_WITH_KNOTS('',3,(#16479,#16480,#16481,#16482),
 .UNSPECIFIED.,.F.,.F.,(4,4),(1.622093506599E-14,0.000408584946011366),
 .UNSPECIFIED.);
#873=B_SPLINE_CURVE_WITH_KNOTS('',3,(#16484,#16485,#16486,#16487),
 .UNSPECIFIED.,.F.,.F.,(4,4),(0.,1.),.UNSPECIFIED.);
#874=B_SPLINE_CURVE_WITH_KNOTS('',3,(#16489,#16490,#16491,#16492),
 .UNSPECIFIED.,.F.,.F.,(4,4),(8.75998893489131E-10,0.000408584945827489),
 .UNSPECIFIED.);
#875=B_SPLINE_CURVE_WITH_KNOTS('',3,(#16494,#16495,#16496,#16497),
 .UNSPECIFIED.,.F.,.F.,(4,4),(0.,1.),.UNSPECIFIED.);
#876=B_SPLINE_CURVE_WITH_KNOTS('',3,(#16499,#16500,#16501,#16502),
 .UNSPECIFIED.,.F.,.F.,(4,4),(0.,1.),.UNSPECIFIED.);
#877=B_SPLINE_CURVE_WITH_KNOTS('',3,(#16504,#16505,#16506,#16507),
 .UNSPECIFIED.,.F.,.F.,(4,4),(2.1214408803583E-14,0.000408584946680086),
 .UNSPECIFIED.);
#878=B_SPLINE_CURVE_WITH_KNOTS('',3,(#16509,#16510,#16511,#16512),
 .UNSPECIFIED.,.F.,.F.,(4,4),(0.,1.),.UNSPECIFIED.);
#879=B_SPLINE_CURVE_WITH_KNOTS('',3,(#16514,#16515,#16516,#16517),
 .UNSPECIFIED.,.F.,.F.,(4,4),(8.72748227154931E-10,0.000408584950442943),
 .UNSPECIFIED.);
#880=B_SPLINE_CURVE_WITH_KNOTS('',3,(#16519,#16520,#16521,#16522),
 .UNSPECIFIED.,.F.,.F.,(4,4),(0.,1.),.UNSPECIFIED.);
#881=B_SPLINE_CURVE_WITH_KNOTS('',3,(#16524,#16525,#16526,#16527),
 .UNSPECIFIED.,.F.,.F.,(4,4),(0.,1.),.UNSPECIFIED.);
#882=B_SPLINE_CURVE_WITH_KNOTS('',3,(#16529,#16530,#16531,#16532),
 .UNSPECIFIED.,.F.,.F.,(4,4),(6.86945077261581E-14,0.000408584947563837),
 .UNSPECIFIED.);
#883=B_SPLINE_CURVE_WITH_KNOTS('',3,(#16534,#16535,#16536,#16537),
 .UNSPECIFIED.,.F.,.F.,(4,4),(5.9410360424763E-7,1.),.UNSPECIFIED.);
#884=B_SPLINE_CURVE_WITH_KNOTS('',3,(#16539,#16540,#16541,#16542),
 .UNSPECIFIED.,.F.,.F.,(4,4),(8.73453709605601E-10,0.000408584949164257),
 .UNSPECIFIED.);
#885=B_SPLINE_CURVE_WITH_KNOTS('',3,(#16544,#16545,#16546,#16547),
 .UNSPECIFIED.,.F.,.F.,(4,4),(0.,0.999999400915229),.UNSPECIFIED.);
#886=B_SPLINE_CURVE_WITH_KNOTS('',3,(#16549,#16550,#16551,#16552),
 .UNSPECIFIED.,.F.,.F.,(4,4),(0.,1.),.UNSPECIFIED.);
#887=B_SPLINE_CURVE_WITH_KNOTS('',3,(#17303,#17304,#17305,#17306),
 .UNSPECIFIED.,.F.,.F.,(4,4),(0.,0.000408585662909977),.UNSPECIFIED.);
#888=PLANE('',#8243);
#889=PLANE('',#8245);
#890=PLANE('',#8290);
#891=PLANE('',#8292);
#892=PLANE('',#8293);
#893=PLANE('',#8295);
#894=PLANE('',#8296);
#895=PLANE('',#8298);
#896=PLANE('',#8299);
#897=PLANE('',#8301);
#898=PLANE('',#8302);
#899=PLANE('',#8304);
#900=PLANE('',#8305);
#901=PLANE('',#8307);
#902=PLANE('',#8308);
#903=PLANE('',#8310);
#904=PLANE('',#8311);
#905=PLANE('',#8313);
#906=PLANE('',#8314);
#907=PLANE('',#8316);
#908=PLANE('',#8317);
#909=PLANE('',#8319);
#910=PLANE('',#8320);
#911=PLANE('',#8322);
#912=PLANE('',#8323);
#913=PLANE('',#8325);
#914=PLANE('',#8326);
#915=PLANE('',#8328);
#916=PLANE('',#8329);
#917=PLANE('',#8331);
#918=PLANE('',#8332);
#919=PLANE('',#8334);
#920=PLANE('',#8335);
#921=PLANE('',#8337);
#922=PLANE('',#8338);
#923=PLANE('',#8340);
#924=PLANE('',#8341);
#925=PLANE('',#8343);
#926=PLANE('',#8344);
#927=PLANE('',#8346);
#928=PLANE('',#8347);
#929=PLANE('',#8349);
#930=PLANE('',#8350);
#931=PLANE('',#8352);
#932=PLANE('',#8353);
#933=PLANE('',#8355);
#934=PLANE('',#8356);
#935=PLANE('',#8358);
#936=PLANE('',#8359);
#937=PLANE('',#8361);
#938=PLANE('',#8362);
#939=PLANE('',#8364);
#940=PLANE('',#8365);
#941=PLANE('',#8367);
#942=PLANE('',#8368);
#943=PLANE('',#8370);
#944=PLANE('',#8371);
#945=PLANE('',#8373);
#946=PLANE('',#8374);
#947=PLANE('',#8376);
#948=PLANE('',#8377);
#949=PLANE('',#8379);
#950=PLANE('',#8380);
#951=PLANE('',#8382);
#952=PLANE('',#8383);
#953=PLANE('',#8385);
#954=PLANE('',#8386);
#955=PLANE('',#8388);
#956=PLANE('',#8389);
#957=PLANE('',#8391);
#958=PLANE('',#8392);
#959=PLANE('',#8394);
#960=PLANE('',#8395);
#961=PLANE('',#8397);
#962=PLANE('',#8398);
#963=PLANE('',#8400);
#964=PLANE('',#8401);
#965=PLANE('',#8403);
#966=PLANE('',#8404);
#967=PLANE('',#8406);
#968=PLANE('',#8407);
#969=PLANE('',#8409);
#970=PLANE('',#8410);
#971=PLANE('',#8414);
#972=PLANE('',#8415);
#973=PLANE('',#8440);
#974=PLANE('',#8441);
#975=PLANE('',#8444);
#976=PLANE('',#8445);
#977=PLANE('',#8448);
#978=PLANE('',#8449);
#979=PLANE('',#8452);
#980=PLANE('',#8453);
#981=PLANE('',#8456);
#982=PLANE('',#8457);
#983=PLANE('',#8460);
#984=PLANE('',#8461);
#985=PLANE('',#8464);
#986=PLANE('',#8465);
#987=PLANE('',#8468);
#988=PLANE('',#8469);
#989=PLANE('',#8472);
#990=PLANE('',#8473);
#991=PLANE('',#8476);
#992=PLANE('',#8477);
#993=PLANE('',#8480);
#994=PLANE('',#8481);
#995=PLANE('',#8484);
#996=PLANE('',#8485);
#997=PLANE('',#8488);
#998=PLANE('',#8489);
#999=PLANE('',#8492);
#1000=PLANE('',#8493);
#1001=PLANE('',#8496);
#1002=PLANE('',#8497);
#1003=PLANE('',#8500);
#1004=PLANE('',#8501);
#1005=PLANE('',#8504);
#1006=PLANE('',#8505);
#1007=PLANE('',#8508);
#1008=PLANE('',#8509);
#1009=PLANE('',#8512);
#1010=PLANE('',#8513);
#1011=PLANE('',#8516);
#1012=PLANE('',#8517);
#1013=PLANE('',#8518);
#1014=PLANE('',#8520);
#1015=PLANE('',#8521);
#1016=PLANE('',#8522);
#1017=PLANE('',#8523);
#1018=PLANE('',#8524);
#1019=PLANE('',#8525);
#1020=PLANE('',#8526);
#1021=PLANE('',#8527);
#1022=PLANE('',#8528);
#1023=PLANE('',#8529);
#1024=PLANE('',#8530);
#1025=PLANE('',#8531);
#1026=PLANE('',#8532);
#1027=PLANE('',#8533);
#1028=PLANE('',#8534);
#1029=PLANE('',#8535);
#1030=PLANE('',#8536);
#1031=PLANE('',#8537);
#1032=PLANE('',#8538);
#1033=PLANE('',#8545);
#1034=PLANE('',#8547);
#1035=PLANE('',#8557);
#1036=PLANE('',#8581);
#1037=PLANE('',#8583);
#1038=PLANE('',#8593);
#1039=PLANE('',#8617);
#1040=PLANE('',#8628);
#1041=PLANE('',#8634);
#1042=PLANE('',#8647);
#1043=PLANE('',#8656);
#1044=PLANE('',#8667);
#1045=PLANE('',#8673);
#1046=PLANE('',#8686);
#1047=PLANE('',#8695);
#1048=PLANE('',#8697);
#1049=PLANE('',#8703);
#1050=PLANE('',#8705);
#1051=PLANE('',#8711);
#1052=PLANE('',#8713);
#1053=PLANE('',#8719);
#1054=PLANE('',#8721);
#1055=PLANE('',#8727);
#1056=PLANE('',#8729);
#1057=PLANE('',#8735);
#1058=PLANE('',#8737);
#1059=PLANE('',#8743);
#1060=PLANE('',#8745);
#1061=PLANE('',#8751);
#1062=PLANE('',#8753);
#1063=PLANE('',#8759);
#1064=PLANE('',#8821);
#1065=PLANE('',#8834);
#1066=PLANE('',#8879);
#1067=PLANE('',#8886);
#1068=PLANE('',#8969);
#1069=PLANE('',#9008);
#1070=PLANE('',#9027);
#1071=PLANE('',#9031);
#1072=PLANE('',#9032);
#1073=PLANE('',#9036);
#1074=PLANE('',#9040);
#1075=PLANE('',#9041);
#1076=PLANE('',#9045);
#1077=PLANE('',#9046);
#1078=PLANE('',#9050);
#1079=PLANE('',#9051);
#1080=PLANE('',#9055);
#1081=PLANE('',#9069);
#1082=PLANE('',#9112);
#1083=PLANE('',#9114);
#1084=PLANE('',#9116);
#1085=PLANE('',#9118);
#1086=PLANE('',#9125);
#1087=PLANE('',#9127);
#1088=PLANE('',#9129);
#1089=PLANE('',#9131);
#1090=PLANE('',#9133);
#1091=PLANE('',#9135);
#1092=PLANE('',#9137);
#1093=PLANE('',#9142);
#1094=ORIENTED_EDGE('',*,*,#3468,.F.);
#1095=ORIENTED_EDGE('',*,*,#3469,.F.);
#1096=ORIENTED_EDGE('',*,*,#3470,.F.);
#1097=ORIENTED_EDGE('',*,*,#3468,.T.);
#1098=ORIENTED_EDGE('',*,*,#3471,.F.);
#1099=ORIENTED_EDGE('',*,*,#3469,.T.);
#1100=ORIENTED_EDGE('',*,*,#3470,.T.);
#1101=ORIENTED_EDGE('',*,*,#3472,.T.);
#1102=ORIENTED_EDGE('',*,*,#3473,.T.);
#1103=ORIENTED_EDGE('',*,*,#3474,.T.);
#1104=ORIENTED_EDGE('',*,*,#3475,.T.);
#1105=ORIENTED_EDGE('',*,*,#3476,.T.);
#1106=ORIENTED_EDGE('',*,*,#3477,.T.);
#1107=ORIENTED_EDGE('',*,*,#3478,.T.);
#1108=ORIENTED_EDGE('',*,*,#3479,.T.);
#1109=ORIENTED_EDGE('',*,*,#3480,.T.);
#1110=ORIENTED_EDGE('',*,*,#3481,.T.);
#1111=ORIENTED_EDGE('',*,*,#3482,.T.);
#1112=ORIENTED_EDGE('',*,*,#3483,.T.);
#1113=ORIENTED_EDGE('',*,*,#3484,.T.);
#1114=ORIENTED_EDGE('',*,*,#3485,.T.);
#1115=ORIENTED_EDGE('',*,*,#3486,.T.);
#1116=ORIENTED_EDGE('',*,*,#3487,.T.);
#1117=ORIENTED_EDGE('',*,*,#3488,.T.);
#1118=ORIENTED_EDGE('',*,*,#3489,.T.);
#1119=ORIENTED_EDGE('',*,*,#3490,.T.);
#1120=ORIENTED_EDGE('',*,*,#3491,.T.);
#1121=ORIENTED_EDGE('',*,*,#3492,.T.);
#1122=ORIENTED_EDGE('',*,*,#3493,.T.);
#1123=ORIENTED_EDGE('',*,*,#3494,.T.);
#1124=ORIENTED_EDGE('',*,*,#3495,.T.);
#1125=ORIENTED_EDGE('',*,*,#3496,.T.);
#1126=ORIENTED_EDGE('',*,*,#3497,.T.);
#1127=ORIENTED_EDGE('',*,*,#3498,.T.);
#1128=ORIENTED_EDGE('',*,*,#3499,.T.);
#1129=ORIENTED_EDGE('',*,*,#3500,.T.);
#1130=ORIENTED_EDGE('',*,*,#3501,.T.);
#1131=ORIENTED_EDGE('',*,*,#3502,.T.);
#1132=ORIENTED_EDGE('',*,*,#3503,.T.);
#1133=ORIENTED_EDGE('',*,*,#3504,.T.);
#1134=ORIENTED_EDGE('',*,*,#3505,.T.);
#1135=ORIENTED_EDGE('',*,*,#3506,.T.);
#1136=ORIENTED_EDGE('',*,*,#3507,.T.);
#1137=ORIENTED_EDGE('',*,*,#3508,.T.);
#1138=ORIENTED_EDGE('',*,*,#3509,.T.);
#1139=ORIENTED_EDGE('',*,*,#3510,.T.);
#1140=ORIENTED_EDGE('',*,*,#3511,.T.);
#1141=ORIENTED_EDGE('',*,*,#3512,.T.);
#1142=ORIENTED_EDGE('',*,*,#3513,.T.);
#1143=ORIENTED_EDGE('',*,*,#3514,.T.);
#1144=ORIENTED_EDGE('',*,*,#3515,.T.);
#1145=ORIENTED_EDGE('',*,*,#3516,.T.);
#1146=ORIENTED_EDGE('',*,*,#3517,.T.);
#1147=ORIENTED_EDGE('',*,*,#3518,.T.);
#1148=ORIENTED_EDGE('',*,*,#3519,.T.);
#1149=ORIENTED_EDGE('',*,*,#3520,.T.);
#1150=ORIENTED_EDGE('',*,*,#3521,.T.);
#1151=ORIENTED_EDGE('',*,*,#3522,.T.);
#1152=ORIENTED_EDGE('',*,*,#3523,.T.);
#1153=ORIENTED_EDGE('',*,*,#3524,.T.);
#1154=ORIENTED_EDGE('',*,*,#3525,.T.);
#1155=ORIENTED_EDGE('',*,*,#3526,.T.);
#1156=ORIENTED_EDGE('',*,*,#3527,.T.);
#1157=ORIENTED_EDGE('',*,*,#3528,.T.);
#1158=ORIENTED_EDGE('',*,*,#3529,.T.);
#1159=ORIENTED_EDGE('',*,*,#3530,.T.);
#1160=ORIENTED_EDGE('',*,*,#3531,.T.);
#1161=ORIENTED_EDGE('',*,*,#3532,.T.);
#1162=ORIENTED_EDGE('',*,*,#3533,.T.);
#1163=ORIENTED_EDGE('',*,*,#3534,.T.);
#1164=ORIENTED_EDGE('',*,*,#3535,.T.);
#1165=ORIENTED_EDGE('',*,*,#3536,.T.);
#1166=ORIENTED_EDGE('',*,*,#3537,.T.);
#1167=ORIENTED_EDGE('',*,*,#3538,.T.);
#1168=ORIENTED_EDGE('',*,*,#3539,.T.);
#1169=ORIENTED_EDGE('',*,*,#3540,.T.);
#1170=ORIENTED_EDGE('',*,*,#3541,.T.);
#1171=ORIENTED_EDGE('',*,*,#3542,.T.);
#1172=ORIENTED_EDGE('',*,*,#3543,.T.);
#1173=ORIENTED_EDGE('',*,*,#3544,.T.);
#1174=ORIENTED_EDGE('',*,*,#3545,.T.);
#1175=ORIENTED_EDGE('',*,*,#3546,.T.);
#1176=ORIENTED_EDGE('',*,*,#3547,.T.);
#1177=ORIENTED_EDGE('',*,*,#3548,.T.);
#1178=ORIENTED_EDGE('',*,*,#3549,.T.);
#1179=ORIENTED_EDGE('',*,*,#3550,.T.);
#1180=ORIENTED_EDGE('',*,*,#3551,.T.);
#1181=ORIENTED_EDGE('',*,*,#3552,.T.);
#1182=ORIENTED_EDGE('',*,*,#3471,.T.);
#1183=ORIENTED_EDGE('',*,*,#3512,.F.);
#1184=ORIENTED_EDGE('',*,*,#3553,.T.);
#1185=ORIENTED_EDGE('',*,*,#3554,.T.);
#1186=ORIENTED_EDGE('',*,*,#3555,.T.);
#1187=ORIENTED_EDGE('',*,*,#3513,.F.);
#1188=ORIENTED_EDGE('',*,*,#3555,.F.);
#1189=ORIENTED_EDGE('',*,*,#3556,.T.);
#1190=ORIENTED_EDGE('',*,*,#3557,.T.);
#1191=ORIENTED_EDGE('',*,*,#3558,.T.);
#1192=ORIENTED_EDGE('',*,*,#3559,.F.);
#1193=ORIENTED_EDGE('',*,*,#3560,.F.);
#1194=ORIENTED_EDGE('',*,*,#3561,.F.);
#1195=ORIENTED_EDGE('',*,*,#3514,.F.);
#1196=ORIENTED_EDGE('',*,*,#3558,.F.);
#1197=ORIENTED_EDGE('',*,*,#3562,.F.);
#1198=ORIENTED_EDGE('',*,*,#3563,.T.);
#1199=ORIENTED_EDGE('',*,*,#3564,.T.);
#1200=ORIENTED_EDGE('',*,*,#3565,.T.);
#1201=ORIENTED_EDGE('',*,*,#3515,.F.);
#1202=ORIENTED_EDGE('',*,*,#3561,.T.);
#1203=ORIENTED_EDGE('',*,*,#3516,.F.);
#1204=ORIENTED_EDGE('',*,*,#3565,.F.);
#1205=ORIENTED_EDGE('',*,*,#3566,.T.);
#1206=ORIENTED_EDGE('',*,*,#3567,.T.);
#1207=ORIENTED_EDGE('',*,*,#3517,.F.);
#1208=ORIENTED_EDGE('',*,*,#3567,.F.);
#1209=ORIENTED_EDGE('',*,*,#3568,.T.);
#1210=ORIENTED_EDGE('',*,*,#3569,.T.);
#1211=ORIENTED_EDGE('',*,*,#3570,.T.);
#1212=ORIENTED_EDGE('',*,*,#3570,.F.);
#1213=ORIENTED_EDGE('',*,*,#3571,.F.);
#1214=ORIENTED_EDGE('',*,*,#3572,.F.);
#1215=ORIENTED_EDGE('',*,*,#3573,.F.);
#1216=ORIENTED_EDGE('',*,*,#3574,.F.);
#1217=ORIENTED_EDGE('',*,*,#3518,.F.);
#1218=ORIENTED_EDGE('',*,*,#3575,.T.);
#1219=ORIENTED_EDGE('',*,*,#3576,.T.);
#1220=ORIENTED_EDGE('',*,*,#3577,.T.);
#1221=ORIENTED_EDGE('',*,*,#3519,.F.);
#1222=ORIENTED_EDGE('',*,*,#3574,.T.);
#1223=ORIENTED_EDGE('',*,*,#3520,.F.);
#1224=ORIENTED_EDGE('',*,*,#3577,.F.);
#1225=ORIENTED_EDGE('',*,*,#3578,.T.);
#1226=ORIENTED_EDGE('',*,*,#3579,.T.);
#1227=ORIENTED_EDGE('',*,*,#3521,.F.);
#1228=ORIENTED_EDGE('',*,*,#3579,.F.);
#1229=ORIENTED_EDGE('',*,*,#3580,.T.);
#1230=ORIENTED_EDGE('',*,*,#3581,.T.);
#1231=ORIENTED_EDGE('',*,*,#3582,.T.);
#1232=ORIENTED_EDGE('',*,*,#3582,.F.);
#1233=ORIENTED_EDGE('',*,*,#3583,.F.);
#1234=ORIENTED_EDGE('',*,*,#3584,.F.);
#1235=ORIENTED_EDGE('',*,*,#3585,.F.);
#1236=ORIENTED_EDGE('',*,*,#3586,.F.);
#1237=ORIENTED_EDGE('',*,*,#3522,.F.);
#1238=ORIENTED_EDGE('',*,*,#3587,.T.);
#1239=ORIENTED_EDGE('',*,*,#3588,.T.);
#1240=ORIENTED_EDGE('',*,*,#3589,.T.);
#1241=ORIENTED_EDGE('',*,*,#3523,.F.);
#1242=ORIENTED_EDGE('',*,*,#3586,.T.);
#1243=ORIENTED_EDGE('',*,*,#3524,.F.);
#1244=ORIENTED_EDGE('',*,*,#3589,.F.);
#1245=ORIENTED_EDGE('',*,*,#3590,.T.);
#1246=ORIENTED_EDGE('',*,*,#3591,.T.);
#1247=ORIENTED_EDGE('',*,*,#3525,.F.);
#1248=ORIENTED_EDGE('',*,*,#3591,.F.);
#1249=ORIENTED_EDGE('',*,*,#3592,.T.);
#1250=ORIENTED_EDGE('',*,*,#3593,.T.);
#1251=ORIENTED_EDGE('',*,*,#3594,.T.);
#1252=ORIENTED_EDGE('',*,*,#3594,.F.);
#1253=ORIENTED_EDGE('',*,*,#3595,.F.);
#1254=ORIENTED_EDGE('',*,*,#3596,.F.);
#1255=ORIENTED_EDGE('',*,*,#3597,.F.);
#1256=ORIENTED_EDGE('',*,*,#3598,.F.);
#1257=ORIENTED_EDGE('',*,*,#3526,.F.);
#1258=ORIENTED_EDGE('',*,*,#3599,.T.);
#1259=ORIENTED_EDGE('',*,*,#3600,.T.);
#1260=ORIENTED_EDGE('',*,*,#3601,.T.);
#1261=ORIENTED_EDGE('',*,*,#3527,.F.);
#1262=ORIENTED_EDGE('',*,*,#3598,.T.);
#1263=ORIENTED_EDGE('',*,*,#3528,.F.);
#1264=ORIENTED_EDGE('',*,*,#3601,.F.);
#1265=ORIENTED_EDGE('',*,*,#3602,.T.);
#1266=ORIENTED_EDGE('',*,*,#3603,.T.);
#1267=ORIENTED_EDGE('',*,*,#3529,.F.);
#1268=ORIENTED_EDGE('',*,*,#3603,.F.);
#1269=ORIENTED_EDGE('',*,*,#3604,.T.);
#1270=ORIENTED_EDGE('',*,*,#3605,.T.);
#1271=ORIENTED_EDGE('',*,*,#3606,.T.);
#1272=ORIENTED_EDGE('',*,*,#3606,.F.);
#1273=ORIENTED_EDGE('',*,*,#3607,.F.);
#1274=ORIENTED_EDGE('',*,*,#3608,.F.);
#1275=ORIENTED_EDGE('',*,*,#3609,.F.);
#1276=ORIENTED_EDGE('',*,*,#3610,.F.);
#1277=ORIENTED_EDGE('',*,*,#3530,.F.);
#1278=ORIENTED_EDGE('',*,*,#3611,.T.);
#1279=ORIENTED_EDGE('',*,*,#3612,.T.);
#1280=ORIENTED_EDGE('',*,*,#3613,.T.);
#1281=ORIENTED_EDGE('',*,*,#3531,.F.);
#1282=ORIENTED_EDGE('',*,*,#3610,.T.);
#1283=ORIENTED_EDGE('',*,*,#3532,.F.);
#1284=ORIENTED_EDGE('',*,*,#3613,.F.);
#1285=ORIENTED_EDGE('',*,*,#3614,.T.);
#1286=ORIENTED_EDGE('',*,*,#3615,.T.);
#1287=ORIENTED_EDGE('',*,*,#3533,.F.);
#1288=ORIENTED_EDGE('',*,*,#3615,.F.);
#1289=ORIENTED_EDGE('',*,*,#3616,.T.);
#1290=ORIENTED_EDGE('',*,*,#3617,.T.);
#1291=ORIENTED_EDGE('',*,*,#3618,.T.);
#1292=ORIENTED_EDGE('',*,*,#3618,.F.);
#1293=ORIENTED_EDGE('',*,*,#3619,.F.);
#1294=ORIENTED_EDGE('',*,*,#3620,.F.);
#1295=ORIENTED_EDGE('',*,*,#3621,.F.);
#1296=ORIENTED_EDGE('',*,*,#3622,.F.);
#1297=ORIENTED_EDGE('',*,*,#3534,.F.);
#1298=ORIENTED_EDGE('',*,*,#3623,.T.);
#1299=ORIENTED_EDGE('',*,*,#3624,.T.);
#1300=ORIENTED_EDGE('',*,*,#3625,.T.);
#1301=ORIENTED_EDGE('',*,*,#3535,.F.);
#1302=ORIENTED_EDGE('',*,*,#3622,.T.);
#1303=ORIENTED_EDGE('',*,*,#3536,.F.);
#1304=ORIENTED_EDGE('',*,*,#3625,.F.);
#1305=ORIENTED_EDGE('',*,*,#3626,.T.);
#1306=ORIENTED_EDGE('',*,*,#3627,.T.);
#1307=ORIENTED_EDGE('',*,*,#3537,.F.);
#1308=ORIENTED_EDGE('',*,*,#3627,.F.);
#1309=ORIENTED_EDGE('',*,*,#3628,.T.);
#1310=ORIENTED_EDGE('',*,*,#3629,.T.);
#1311=ORIENTED_EDGE('',*,*,#3630,.T.);
#1312=ORIENTED_EDGE('',*,*,#3630,.F.);
#1313=ORIENTED_EDGE('',*,*,#3631,.F.);
#1314=ORIENTED_EDGE('',*,*,#3632,.F.);
#1315=ORIENTED_EDGE('',*,*,#3633,.F.);
#1316=ORIENTED_EDGE('',*,*,#3634,.F.);
#1317=ORIENTED_EDGE('',*,*,#3538,.F.);
#1318=ORIENTED_EDGE('',*,*,#3635,.T.);
#1319=ORIENTED_EDGE('',*,*,#3636,.T.);
#1320=ORIENTED_EDGE('',*,*,#3637,.T.);
#1321=ORIENTED_EDGE('',*,*,#3539,.F.);
#1322=ORIENTED_EDGE('',*,*,#3634,.T.);
#1323=ORIENTED_EDGE('',*,*,#3540,.F.);
#1324=ORIENTED_EDGE('',*,*,#3637,.F.);
#1325=ORIENTED_EDGE('',*,*,#3638,.T.);
#1326=ORIENTED_EDGE('',*,*,#3639,.T.);
#1327=ORIENTED_EDGE('',*,*,#3541,.F.);
#1328=ORIENTED_EDGE('',*,*,#3639,.F.);
#1329=ORIENTED_EDGE('',*,*,#3640,.T.);
#1330=ORIENTED_EDGE('',*,*,#3641,.T.);
#1331=ORIENTED_EDGE('',*,*,#3642,.T.);
#1332=ORIENTED_EDGE('',*,*,#3642,.F.);
#1333=ORIENTED_EDGE('',*,*,#3643,.F.);
#1334=ORIENTED_EDGE('',*,*,#3644,.F.);
#1335=ORIENTED_EDGE('',*,*,#3645,.F.);
#1336=ORIENTED_EDGE('',*,*,#3646,.F.);
#1337=ORIENTED_EDGE('',*,*,#3542,.F.);
#1338=ORIENTED_EDGE('',*,*,#3647,.T.);
#1339=ORIENTED_EDGE('',*,*,#3648,.T.);
#1340=ORIENTED_EDGE('',*,*,#3649,.T.);
#1341=ORIENTED_EDGE('',*,*,#3543,.F.);
#1342=ORIENTED_EDGE('',*,*,#3646,.T.);
#1343=ORIENTED_EDGE('',*,*,#3544,.F.);
#1344=ORIENTED_EDGE('',*,*,#3649,.F.);
#1345=ORIENTED_EDGE('',*,*,#3650,.T.);
#1346=ORIENTED_EDGE('',*,*,#3651,.T.);
#1347=ORIENTED_EDGE('',*,*,#3545,.F.);
#1348=ORIENTED_EDGE('',*,*,#3651,.F.);
#1349=ORIENTED_EDGE('',*,*,#3652,.T.);
#1350=ORIENTED_EDGE('',*,*,#3653,.T.);
#1351=ORIENTED_EDGE('',*,*,#3654,.T.);
#1352=ORIENTED_EDGE('',*,*,#3654,.F.);
#1353=ORIENTED_EDGE('',*,*,#3655,.F.);
#1354=ORIENTED_EDGE('',*,*,#3656,.F.);
#1355=ORIENTED_EDGE('',*,*,#3657,.F.);
#1356=ORIENTED_EDGE('',*,*,#3658,.F.);
#1357=ORIENTED_EDGE('',*,*,#3546,.F.);
#1358=ORIENTED_EDGE('',*,*,#3659,.T.);
#1359=ORIENTED_EDGE('',*,*,#3660,.T.);
#1360=ORIENTED_EDGE('',*,*,#3661,.T.);
#1361=ORIENTED_EDGE('',*,*,#3547,.F.);
#1362=ORIENTED_EDGE('',*,*,#3658,.T.);
#1363=ORIENTED_EDGE('',*,*,#3548,.F.);
#1364=ORIENTED_EDGE('',*,*,#3661,.F.);
#1365=ORIENTED_EDGE('',*,*,#3662,.T.);
#1366=ORIENTED_EDGE('',*,*,#3663,.T.);
#1367=ORIENTED_EDGE('',*,*,#3549,.F.);
#1368=ORIENTED_EDGE('',*,*,#3663,.F.);
#1369=ORIENTED_EDGE('',*,*,#3664,.T.);
#1370=ORIENTED_EDGE('',*,*,#3665,.T.);
#1371=ORIENTED_EDGE('',*,*,#3666,.T.);
#1372=ORIENTED_EDGE('',*,*,#3666,.F.);
#1373=ORIENTED_EDGE('',*,*,#3667,.F.);
#1374=ORIENTED_EDGE('',*,*,#3668,.F.);
#1375=ORIENTED_EDGE('',*,*,#3669,.F.);
#1376=ORIENTED_EDGE('',*,*,#3670,.F.);
#1377=ORIENTED_EDGE('',*,*,#3550,.F.);
#1378=ORIENTED_EDGE('',*,*,#3671,.T.);
#1379=ORIENTED_EDGE('',*,*,#3672,.T.);
#1380=ORIENTED_EDGE('',*,*,#3673,.T.);
#1381=ORIENTED_EDGE('',*,*,#3551,.F.);
#1382=ORIENTED_EDGE('',*,*,#3670,.T.);
#1383=ORIENTED_EDGE('',*,*,#3472,.F.);
#1384=ORIENTED_EDGE('',*,*,#3673,.F.);
#1385=ORIENTED_EDGE('',*,*,#3674,.T.);
#1386=ORIENTED_EDGE('',*,*,#3675,.T.);
#1387=ORIENTED_EDGE('',*,*,#3473,.F.);
#1388=ORIENTED_EDGE('',*,*,#3675,.F.);
#1389=ORIENTED_EDGE('',*,*,#3676,.T.);
#1390=ORIENTED_EDGE('',*,*,#3677,.T.);
#1391=ORIENTED_EDGE('',*,*,#3678,.T.);
#1392=ORIENTED_EDGE('',*,*,#3678,.F.);
#1393=ORIENTED_EDGE('',*,*,#3679,.F.);
#1394=ORIENTED_EDGE('',*,*,#3680,.F.);
#1395=ORIENTED_EDGE('',*,*,#3681,.F.);
#1396=ORIENTED_EDGE('',*,*,#3682,.F.);
#1397=ORIENTED_EDGE('',*,*,#3474,.F.);
#1398=ORIENTED_EDGE('',*,*,#3683,.T.);
#1399=ORIENTED_EDGE('',*,*,#3684,.T.);
#1400=ORIENTED_EDGE('',*,*,#3685,.T.);
#1401=ORIENTED_EDGE('',*,*,#3475,.F.);
#1402=ORIENTED_EDGE('',*,*,#3682,.T.);
#1403=ORIENTED_EDGE('',*,*,#3476,.F.);
#1404=ORIENTED_EDGE('',*,*,#3685,.F.);
#1405=ORIENTED_EDGE('',*,*,#3686,.T.);
#1406=ORIENTED_EDGE('',*,*,#3687,.T.);
#1407=ORIENTED_EDGE('',*,*,#3477,.F.);
#1408=ORIENTED_EDGE('',*,*,#3687,.F.);
#1409=ORIENTED_EDGE('',*,*,#3688,.T.);
#1410=ORIENTED_EDGE('',*,*,#3689,.T.);
#1411=ORIENTED_EDGE('',*,*,#3690,.T.);
#1412=ORIENTED_EDGE('',*,*,#3690,.F.);
#1413=ORIENTED_EDGE('',*,*,#3691,.F.);
#1414=ORIENTED_EDGE('',*,*,#3692,.F.);
#1415=ORIENTED_EDGE('',*,*,#3693,.F.);
#1416=ORIENTED_EDGE('',*,*,#3694,.F.);
#1417=ORIENTED_EDGE('',*,*,#3478,.F.);
#1418=ORIENTED_EDGE('',*,*,#3695,.T.);
#1419=ORIENTED_EDGE('',*,*,#3696,.T.);
#1420=ORIENTED_EDGE('',*,*,#3697,.T.);
#1421=ORIENTED_EDGE('',*,*,#3479,.F.);
#1422=ORIENTED_EDGE('',*,*,#3694,.T.);
#1423=ORIENTED_EDGE('',*,*,#3480,.F.);
#1424=ORIENTED_EDGE('',*,*,#3697,.F.);
#1425=ORIENTED_EDGE('',*,*,#3698,.T.);
#1426=ORIENTED_EDGE('',*,*,#3699,.T.);
#1427=ORIENTED_EDGE('',*,*,#3481,.F.);
#1428=ORIENTED_EDGE('',*,*,#3699,.F.);
#1429=ORIENTED_EDGE('',*,*,#3700,.T.);
#1430=ORIENTED_EDGE('',*,*,#3701,.T.);
#1431=ORIENTED_EDGE('',*,*,#3702,.T.);
#1432=ORIENTED_EDGE('',*,*,#3702,.F.);
#1433=ORIENTED_EDGE('',*,*,#3703,.F.);
#1434=ORIENTED_EDGE('',*,*,#3704,.F.);
#1435=ORIENTED_EDGE('',*,*,#3705,.F.);
#1436=ORIENTED_EDGE('',*,*,#3706,.F.);
#1437=ORIENTED_EDGE('',*,*,#3482,.F.);
#1438=ORIENTED_EDGE('',*,*,#3707,.T.);
#1439=ORIENTED_EDGE('',*,*,#3708,.T.);
#1440=ORIENTED_EDGE('',*,*,#3709,.T.);
#1441=ORIENTED_EDGE('',*,*,#3483,.F.);
#1442=ORIENTED_EDGE('',*,*,#3706,.T.);
#1443=ORIENTED_EDGE('',*,*,#3484,.F.);
#1444=ORIENTED_EDGE('',*,*,#3709,.F.);
#1445=ORIENTED_EDGE('',*,*,#3710,.T.);
#1446=ORIENTED_EDGE('',*,*,#3711,.T.);
#1447=ORIENTED_EDGE('',*,*,#3485,.F.);
#1448=ORIENTED_EDGE('',*,*,#3711,.F.);
#1449=ORIENTED_EDGE('',*,*,#3712,.T.);
#1450=ORIENTED_EDGE('',*,*,#3713,.T.);
#1451=ORIENTED_EDGE('',*,*,#3714,.T.);
#1452=ORIENTED_EDGE('',*,*,#3714,.F.);
#1453=ORIENTED_EDGE('',*,*,#3715,.F.);
#1454=ORIENTED_EDGE('',*,*,#3716,.F.);
#1455=ORIENTED_EDGE('',*,*,#3717,.F.);
#1456=ORIENTED_EDGE('',*,*,#3718,.F.);
#1457=ORIENTED_EDGE('',*,*,#3486,.F.);
#1458=ORIENTED_EDGE('',*,*,#3719,.T.);
#1459=ORIENTED_EDGE('',*,*,#3720,.T.);
#1460=ORIENTED_EDGE('',*,*,#3721,.T.);
#1461=ORIENTED_EDGE('',*,*,#3487,.F.);
#1462=ORIENTED_EDGE('',*,*,#3718,.T.);
#1463=ORIENTED_EDGE('',*,*,#3488,.F.);
#1464=ORIENTED_EDGE('',*,*,#3721,.F.);
#1465=ORIENTED_EDGE('',*,*,#3722,.T.);
#1466=ORIENTED_EDGE('',*,*,#3723,.T.);
#1467=ORIENTED_EDGE('',*,*,#3489,.F.);
#1468=ORIENTED_EDGE('',*,*,#3723,.F.);
#1469=ORIENTED_EDGE('',*,*,#3724,.T.);
#1470=ORIENTED_EDGE('',*,*,#3725,.T.);
#1471=ORIENTED_EDGE('',*,*,#3726,.T.);
#1472=ORIENTED_EDGE('',*,*,#3726,.F.);
#1473=ORIENTED_EDGE('',*,*,#3727,.F.);
#1474=ORIENTED_EDGE('',*,*,#3728,.F.);
#1475=ORIENTED_EDGE('',*,*,#3729,.F.);
#1476=ORIENTED_EDGE('',*,*,#3730,.F.);
#1477=ORIENTED_EDGE('',*,*,#3490,.F.);
#1478=ORIENTED_EDGE('',*,*,#3731,.T.);
#1479=ORIENTED_EDGE('',*,*,#3732,.T.);
#1480=ORIENTED_EDGE('',*,*,#3733,.T.);
#1481=ORIENTED_EDGE('',*,*,#3491,.F.);
#1482=ORIENTED_EDGE('',*,*,#3730,.T.);
#1483=ORIENTED_EDGE('',*,*,#3492,.F.);
#1484=ORIENTED_EDGE('',*,*,#3733,.F.);
#1485=ORIENTED_EDGE('',*,*,#3734,.T.);
#1486=ORIENTED_EDGE('',*,*,#3735,.T.);
#1487=ORIENTED_EDGE('',*,*,#3493,.F.);
#1488=ORIENTED_EDGE('',*,*,#3735,.F.);
#1489=ORIENTED_EDGE('',*,*,#3736,.T.);
#1490=ORIENTED_EDGE('',*,*,#3737,.T.);
#1491=ORIENTED_EDGE('',*,*,#3738,.T.);
#1492=ORIENTED_EDGE('',*,*,#3738,.F.);
#1493=ORIENTED_EDGE('',*,*,#3739,.F.);
#1494=ORIENTED_EDGE('',*,*,#3740,.F.);
#1495=ORIENTED_EDGE('',*,*,#3741,.F.);
#1496=ORIENTED_EDGE('',*,*,#3742,.F.);
#1497=ORIENTED_EDGE('',*,*,#3494,.F.);
#1498=ORIENTED_EDGE('',*,*,#3743,.T.);
#1499=ORIENTED_EDGE('',*,*,#3744,.T.);
#1500=ORIENTED_EDGE('',*,*,#3745,.T.);
#1501=ORIENTED_EDGE('',*,*,#3495,.F.);
#1502=ORIENTED_EDGE('',*,*,#3742,.T.);
#1503=ORIENTED_EDGE('',*,*,#3496,.F.);
#1504=ORIENTED_EDGE('',*,*,#3745,.F.);
#1505=ORIENTED_EDGE('',*,*,#3746,.T.);
#1506=ORIENTED_EDGE('',*,*,#3747,.T.);
#1507=ORIENTED_EDGE('',*,*,#3497,.F.);
#1508=ORIENTED_EDGE('',*,*,#3747,.F.);
#1509=ORIENTED_EDGE('',*,*,#3748,.T.);
#1510=ORIENTED_EDGE('',*,*,#3749,.T.);
#1511=ORIENTED_EDGE('',*,*,#3750,.T.);
#1512=ORIENTED_EDGE('',*,*,#3750,.F.);
#1513=ORIENTED_EDGE('',*,*,#3751,.F.);
#1514=ORIENTED_EDGE('',*,*,#3752,.F.);
#1515=ORIENTED_EDGE('',*,*,#3753,.F.);
#1516=ORIENTED_EDGE('',*,*,#3754,.F.);
#1517=ORIENTED_EDGE('',*,*,#3498,.F.);
#1518=ORIENTED_EDGE('',*,*,#3755,.T.);
#1519=ORIENTED_EDGE('',*,*,#3756,.T.);
#1520=ORIENTED_EDGE('',*,*,#3757,.T.);
#1521=ORIENTED_EDGE('',*,*,#3499,.F.);
#1522=ORIENTED_EDGE('',*,*,#3754,.T.);
#1523=ORIENTED_EDGE('',*,*,#3500,.F.);
#1524=ORIENTED_EDGE('',*,*,#3757,.F.);
#1525=ORIENTED_EDGE('',*,*,#3758,.T.);
#1526=ORIENTED_EDGE('',*,*,#3759,.T.);
#1527=ORIENTED_EDGE('',*,*,#3501,.F.);
#1528=ORIENTED_EDGE('',*,*,#3759,.F.);
#1529=ORIENTED_EDGE('',*,*,#3760,.T.);
#1530=ORIENTED_EDGE('',*,*,#3761,.T.);
#1531=ORIENTED_EDGE('',*,*,#3762,.T.);
#1532=ORIENTED_EDGE('',*,*,#3762,.F.);
#1533=ORIENTED_EDGE('',*,*,#3763,.F.);
#1534=ORIENTED_EDGE('',*,*,#3764,.F.);
#1535=ORIENTED_EDGE('',*,*,#3765,.F.);
#1536=ORIENTED_EDGE('',*,*,#3766,.F.);
#1537=ORIENTED_EDGE('',*,*,#3502,.F.);
#1538=ORIENTED_EDGE('',*,*,#3767,.T.);
#1539=ORIENTED_EDGE('',*,*,#3768,.T.);
#1540=ORIENTED_EDGE('',*,*,#3769,.T.);
#1541=ORIENTED_EDGE('',*,*,#3503,.F.);
#1542=ORIENTED_EDGE('',*,*,#3766,.T.);
#1543=ORIENTED_EDGE('',*,*,#3504,.F.);
#1544=ORIENTED_EDGE('',*,*,#3769,.F.);
#1545=ORIENTED_EDGE('',*,*,#3770,.T.);
#1546=ORIENTED_EDGE('',*,*,#3771,.T.);
#1547=ORIENTED_EDGE('',*,*,#3505,.F.);
#1548=ORIENTED_EDGE('',*,*,#3771,.F.);
#1549=ORIENTED_EDGE('',*,*,#3772,.T.);
#1550=ORIENTED_EDGE('',*,*,#3773,.T.);
#1551=ORIENTED_EDGE('',*,*,#3774,.T.);
#1552=ORIENTED_EDGE('',*,*,#3774,.F.);
#1553=ORIENTED_EDGE('',*,*,#3775,.F.);
#1554=ORIENTED_EDGE('',*,*,#3776,.F.);
#1555=ORIENTED_EDGE('',*,*,#3777,.F.);
#1556=ORIENTED_EDGE('',*,*,#3778,.F.);
#1557=ORIENTED_EDGE('',*,*,#3506,.F.);
#1558=ORIENTED_EDGE('',*,*,#3779,.T.);
#1559=ORIENTED_EDGE('',*,*,#3780,.T.);
#1560=ORIENTED_EDGE('',*,*,#3781,.T.);
#1561=ORIENTED_EDGE('',*,*,#3507,.F.);
#1562=ORIENTED_EDGE('',*,*,#3778,.T.);
#1563=ORIENTED_EDGE('',*,*,#3508,.F.);
#1564=ORIENTED_EDGE('',*,*,#3781,.F.);
#1565=ORIENTED_EDGE('',*,*,#3782,.T.);
#1566=ORIENTED_EDGE('',*,*,#3783,.T.);
#1567=ORIENTED_EDGE('',*,*,#3509,.F.);
#1568=ORIENTED_EDGE('',*,*,#3783,.F.);
#1569=ORIENTED_EDGE('',*,*,#3784,.T.);
#1570=ORIENTED_EDGE('',*,*,#3785,.T.);
#1571=ORIENTED_EDGE('',*,*,#3786,.T.);
#1572=ORIENTED_EDGE('',*,*,#3786,.F.);
#1573=ORIENTED_EDGE('',*,*,#3787,.F.);
#1574=ORIENTED_EDGE('',*,*,#3788,.F.);
#1575=ORIENTED_EDGE('',*,*,#3789,.F.);
#1576=ORIENTED_EDGE('',*,*,#3790,.F.);
#1577=ORIENTED_EDGE('',*,*,#3510,.F.);
#1578=ORIENTED_EDGE('',*,*,#3791,.T.);
#1579=ORIENTED_EDGE('',*,*,#3792,.T.);
#1580=ORIENTED_EDGE('',*,*,#3553,.F.);
#1581=ORIENTED_EDGE('',*,*,#3511,.F.);
#1582=ORIENTED_EDGE('',*,*,#3790,.T.);
#1583=ORIENTED_EDGE('',*,*,#3793,.F.);
#1584=ORIENTED_EDGE('',*,*,#3552,.F.);
#1585=ORIENTED_EDGE('',*,*,#3554,.F.);
#1586=ORIENTED_EDGE('',*,*,#3792,.F.);
#1587=ORIENTED_EDGE('',*,*,#3794,.T.);
#1588=ORIENTED_EDGE('',*,*,#3556,.F.);
#1589=ORIENTED_EDGE('',*,*,#3795,.F.);
#1590=ORIENTED_EDGE('',*,*,#3562,.T.);
#1591=ORIENTED_EDGE('',*,*,#3557,.F.);
#1592=ORIENTED_EDGE('',*,*,#3796,.F.);
#1593=ORIENTED_EDGE('',*,*,#3563,.F.);
#1594=ORIENTED_EDGE('',*,*,#3560,.T.);
#1595=ORIENTED_EDGE('',*,*,#3797,.F.);
#1596=ORIENTED_EDGE('',*,*,#3798,.F.);
#1597=ORIENTED_EDGE('',*,*,#3799,.T.);
#1598=ORIENTED_EDGE('',*,*,#3800,.T.);
#1599=ORIENTED_EDGE('',*,*,#3801,.T.);
#1600=ORIENTED_EDGE('',*,*,#3668,.T.);
#1601=ORIENTED_EDGE('',*,*,#3802,.T.);
#1602=ORIENTED_EDGE('',*,*,#3803,.T.);
#1603=ORIENTED_EDGE('',*,*,#3804,.T.);
#1604=ORIENTED_EDGE('',*,*,#3656,.T.);
#1605=ORIENTED_EDGE('',*,*,#3805,.T.);
#1606=ORIENTED_EDGE('',*,*,#3806,.T.);
#1607=ORIENTED_EDGE('',*,*,#3807,.T.);
#1608=ORIENTED_EDGE('',*,*,#3644,.T.);
#1609=ORIENTED_EDGE('',*,*,#3808,.T.);
#1610=ORIENTED_EDGE('',*,*,#3809,.T.);
#1611=ORIENTED_EDGE('',*,*,#3810,.T.);
#1612=ORIENTED_EDGE('',*,*,#3632,.T.);
#1613=ORIENTED_EDGE('',*,*,#3811,.T.);
#1614=ORIENTED_EDGE('',*,*,#3812,.T.);
#1615=ORIENTED_EDGE('',*,*,#3813,.T.);
#1616=ORIENTED_EDGE('',*,*,#3620,.T.);
#1617=ORIENTED_EDGE('',*,*,#3814,.T.);
#1618=ORIENTED_EDGE('',*,*,#3815,.T.);
#1619=ORIENTED_EDGE('',*,*,#3816,.T.);
#1620=ORIENTED_EDGE('',*,*,#3608,.T.);
#1621=ORIENTED_EDGE('',*,*,#3817,.T.);
#1622=ORIENTED_EDGE('',*,*,#3818,.T.);
#1623=ORIENTED_EDGE('',*,*,#3819,.T.);
#1624=ORIENTED_EDGE('',*,*,#3596,.T.);
#1625=ORIENTED_EDGE('',*,*,#3820,.T.);
#1626=ORIENTED_EDGE('',*,*,#3821,.T.);
#1627=ORIENTED_EDGE('',*,*,#3822,.T.);
#1628=ORIENTED_EDGE('',*,*,#3584,.T.);
#1629=ORIENTED_EDGE('',*,*,#3823,.T.);
#1630=ORIENTED_EDGE('',*,*,#3824,.T.);
#1631=ORIENTED_EDGE('',*,*,#3825,.T.);
#1632=ORIENTED_EDGE('',*,*,#3572,.T.);
#1633=ORIENTED_EDGE('',*,*,#3826,.T.);
#1634=ORIENTED_EDGE('',*,*,#3827,.T.);
#1635=ORIENTED_EDGE('',*,*,#3797,.T.);
#1636=ORIENTED_EDGE('',*,*,#3559,.T.);
#1637=ORIENTED_EDGE('',*,*,#3795,.T.);
#1638=ORIENTED_EDGE('',*,*,#3828,.T.);
#1639=ORIENTED_EDGE('',*,*,#3829,.T.);
#1640=ORIENTED_EDGE('',*,*,#3788,.T.);
#1641=ORIENTED_EDGE('',*,*,#3830,.T.);
#1642=ORIENTED_EDGE('',*,*,#3831,.T.);
#1643=ORIENTED_EDGE('',*,*,#3832,.T.);
#1644=ORIENTED_EDGE('',*,*,#3776,.T.);
#1645=ORIENTED_EDGE('',*,*,#3833,.T.);
#1646=ORIENTED_EDGE('',*,*,#3834,.T.);
#1647=ORIENTED_EDGE('',*,*,#3835,.T.);
#1648=ORIENTED_EDGE('',*,*,#3764,.T.);
#1649=ORIENTED_EDGE('',*,*,#3836,.T.);
#1650=ORIENTED_EDGE('',*,*,#3837,.T.);
#1651=ORIENTED_EDGE('',*,*,#3838,.T.);
#1652=ORIENTED_EDGE('',*,*,#3752,.T.);
#1653=ORIENTED_EDGE('',*,*,#3839,.T.);
#1654=ORIENTED_EDGE('',*,*,#3840,.T.);
#1655=ORIENTED_EDGE('',*,*,#3841,.T.);
#1656=ORIENTED_EDGE('',*,*,#3740,.T.);
#1657=ORIENTED_EDGE('',*,*,#3842,.T.);
#1658=ORIENTED_EDGE('',*,*,#3843,.T.);
#1659=ORIENTED_EDGE('',*,*,#3844,.T.);
#1660=ORIENTED_EDGE('',*,*,#3728,.T.);
#1661=ORIENTED_EDGE('',*,*,#3845,.T.);
#1662=ORIENTED_EDGE('',*,*,#3846,.T.);
#1663=ORIENTED_EDGE('',*,*,#3847,.T.);
#1664=ORIENTED_EDGE('',*,*,#3716,.T.);
#1665=ORIENTED_EDGE('',*,*,#3848,.T.);
#1666=ORIENTED_EDGE('',*,*,#3849,.T.);
#1667=ORIENTED_EDGE('',*,*,#3850,.T.);
#1668=ORIENTED_EDGE('',*,*,#3704,.T.);
#1669=ORIENTED_EDGE('',*,*,#3851,.T.);
#1670=ORIENTED_EDGE('',*,*,#3852,.T.);
#1671=ORIENTED_EDGE('',*,*,#3853,.T.);
#1672=ORIENTED_EDGE('',*,*,#3692,.T.);
#1673=ORIENTED_EDGE('',*,*,#3854,.T.);
#1674=ORIENTED_EDGE('',*,*,#3855,.T.);
#1675=ORIENTED_EDGE('',*,*,#3856,.T.);
#1676=ORIENTED_EDGE('',*,*,#3680,.T.);
#1677=ORIENTED_EDGE('',*,*,#3857,.T.);
#1678=ORIENTED_EDGE('',*,*,#3564,.F.);
#1679=ORIENTED_EDGE('',*,*,#3858,.T.);
#1680=ORIENTED_EDGE('',*,*,#3568,.F.);
#1681=ORIENTED_EDGE('',*,*,#3566,.F.);
#1682=ORIENTED_EDGE('',*,*,#3826,.F.);
#1683=ORIENTED_EDGE('',*,*,#3571,.T.);
#1684=ORIENTED_EDGE('',*,*,#3569,.F.);
#1685=ORIENTED_EDGE('',*,*,#3859,.F.);
#1686=ORIENTED_EDGE('',*,*,#3575,.F.);
#1687=ORIENTED_EDGE('',*,*,#3573,.T.);
#1688=ORIENTED_EDGE('',*,*,#3825,.F.);
#1689=ORIENTED_EDGE('',*,*,#3860,.F.);
#1690=ORIENTED_EDGE('',*,*,#3576,.F.);
#1691=ORIENTED_EDGE('',*,*,#3861,.T.);
#1692=ORIENTED_EDGE('',*,*,#3580,.F.);
#1693=ORIENTED_EDGE('',*,*,#3578,.F.);
#1694=ORIENTED_EDGE('',*,*,#3823,.F.);
#1695=ORIENTED_EDGE('',*,*,#3583,.T.);
#1696=ORIENTED_EDGE('',*,*,#3581,.F.);
#1697=ORIENTED_EDGE('',*,*,#3862,.F.);
#1698=ORIENTED_EDGE('',*,*,#3587,.F.);
#1699=ORIENTED_EDGE('',*,*,#3585,.T.);
#1700=ORIENTED_EDGE('',*,*,#3822,.F.);
#1701=ORIENTED_EDGE('',*,*,#3863,.F.);
#1702=ORIENTED_EDGE('',*,*,#3588,.F.);
#1703=ORIENTED_EDGE('',*,*,#3864,.T.);
#1704=ORIENTED_EDGE('',*,*,#3592,.F.);
#1705=ORIENTED_EDGE('',*,*,#3590,.F.);
#1706=ORIENTED_EDGE('',*,*,#3820,.F.);
#1707=ORIENTED_EDGE('',*,*,#3595,.T.);
#1708=ORIENTED_EDGE('',*,*,#3593,.F.);
#1709=ORIENTED_EDGE('',*,*,#3865,.F.);
#1710=ORIENTED_EDGE('',*,*,#3599,.F.);
#1711=ORIENTED_EDGE('',*,*,#3597,.T.);
#1712=ORIENTED_EDGE('',*,*,#3819,.F.);
#1713=ORIENTED_EDGE('',*,*,#3866,.F.);
#1714=ORIENTED_EDGE('',*,*,#3600,.F.);
#1715=ORIENTED_EDGE('',*,*,#3867,.T.);
#1716=ORIENTED_EDGE('',*,*,#3604,.F.);
#1717=ORIENTED_EDGE('',*,*,#3602,.F.);
#1718=ORIENTED_EDGE('',*,*,#3817,.F.);
#1719=ORIENTED_EDGE('',*,*,#3607,.T.);
#1720=ORIENTED_EDGE('',*,*,#3605,.F.);
#1721=ORIENTED_EDGE('',*,*,#3868,.F.);
#1722=ORIENTED_EDGE('',*,*,#3611,.F.);
#1723=ORIENTED_EDGE('',*,*,#3609,.T.);
#1724=ORIENTED_EDGE('',*,*,#3816,.F.);
#1725=ORIENTED_EDGE('',*,*,#3869,.F.);
#1726=ORIENTED_EDGE('',*,*,#3612,.F.);
#1727=ORIENTED_EDGE('',*,*,#3870,.T.);
#1728=ORIENTED_EDGE('',*,*,#3616,.F.);
#1729=ORIENTED_EDGE('',*,*,#3614,.F.);
#1730=ORIENTED_EDGE('',*,*,#3814,.F.);
#1731=ORIENTED_EDGE('',*,*,#3619,.T.);
#1732=ORIENTED_EDGE('',*,*,#3617,.F.);
#1733=ORIENTED_EDGE('',*,*,#3871,.F.);
#1734=ORIENTED_EDGE('',*,*,#3623,.F.);
#1735=ORIENTED_EDGE('',*,*,#3621,.T.);
#1736=ORIENTED_EDGE('',*,*,#3813,.F.);
#1737=ORIENTED_EDGE('',*,*,#3872,.F.);
#1738=ORIENTED_EDGE('',*,*,#3624,.F.);
#1739=ORIENTED_EDGE('',*,*,#3873,.T.);
#1740=ORIENTED_EDGE('',*,*,#3628,.F.);
#1741=ORIENTED_EDGE('',*,*,#3626,.F.);
#1742=ORIENTED_EDGE('',*,*,#3811,.F.);
#1743=ORIENTED_EDGE('',*,*,#3631,.T.);
#1744=ORIENTED_EDGE('',*,*,#3629,.F.);
#1745=ORIENTED_EDGE('',*,*,#3874,.F.);
#1746=ORIENTED_EDGE('',*,*,#3635,.F.);
#1747=ORIENTED_EDGE('',*,*,#3633,.T.);
#1748=ORIENTED_EDGE('',*,*,#3810,.F.);
#1749=ORIENTED_EDGE('',*,*,#3875,.F.);
#1750=ORIENTED_EDGE('',*,*,#3636,.F.);
#1751=ORIENTED_EDGE('',*,*,#3876,.T.);
#1752=ORIENTED_EDGE('',*,*,#3640,.F.);
#1753=ORIENTED_EDGE('',*,*,#3638,.F.);
#1754=ORIENTED_EDGE('',*,*,#3808,.F.);
#1755=ORIENTED_EDGE('',*,*,#3643,.T.);
#1756=ORIENTED_EDGE('',*,*,#3641,.F.);
#1757=ORIENTED_EDGE('',*,*,#3877,.F.);
#1758=ORIENTED_EDGE('',*,*,#3647,.F.);
#1759=ORIENTED_EDGE('',*,*,#3645,.T.);
#1760=ORIENTED_EDGE('',*,*,#3807,.F.);
#1761=ORIENTED_EDGE('',*,*,#3878,.F.);
#1762=ORIENTED_EDGE('',*,*,#3648,.F.);
#1763=ORIENTED_EDGE('',*,*,#3879,.T.);
#1764=ORIENTED_EDGE('',*,*,#3652,.F.);
#1765=ORIENTED_EDGE('',*,*,#3650,.F.);
#1766=ORIENTED_EDGE('',*,*,#3805,.F.);
#1767=ORIENTED_EDGE('',*,*,#3655,.T.);
#1768=ORIENTED_EDGE('',*,*,#3653,.F.);
#1769=ORIENTED_EDGE('',*,*,#3880,.F.);
#1770=ORIENTED_EDGE('',*,*,#3659,.F.);
#1771=ORIENTED_EDGE('',*,*,#3657,.T.);
#1772=ORIENTED_EDGE('',*,*,#3804,.F.);
#1773=ORIENTED_EDGE('',*,*,#3881,.F.);
#1774=ORIENTED_EDGE('',*,*,#3660,.F.);
#1775=ORIENTED_EDGE('',*,*,#3882,.T.);
#1776=ORIENTED_EDGE('',*,*,#3664,.F.);
#1777=ORIENTED_EDGE('',*,*,#3662,.F.);
#1778=ORIENTED_EDGE('',*,*,#3802,.F.);
#1779=ORIENTED_EDGE('',*,*,#3667,.T.);
#1780=ORIENTED_EDGE('',*,*,#3665,.F.);
#1781=ORIENTED_EDGE('',*,*,#3883,.F.);
#1782=ORIENTED_EDGE('',*,*,#3671,.F.);
#1783=ORIENTED_EDGE('',*,*,#3669,.T.);
#1784=ORIENTED_EDGE('',*,*,#3801,.F.);
#1785=ORIENTED_EDGE('',*,*,#3884,.F.);
#1786=ORIENTED_EDGE('',*,*,#3672,.F.);
#1787=ORIENTED_EDGE('',*,*,#3885,.T.);
#1788=ORIENTED_EDGE('',*,*,#3676,.F.);
#1789=ORIENTED_EDGE('',*,*,#3674,.F.);
#1790=ORIENTED_EDGE('',*,*,#3799,.F.);
#1791=ORIENTED_EDGE('',*,*,#3679,.T.);
#1792=ORIENTED_EDGE('',*,*,#3677,.F.);
#1793=ORIENTED_EDGE('',*,*,#3886,.F.);
#1794=ORIENTED_EDGE('',*,*,#3683,.F.);
#1795=ORIENTED_EDGE('',*,*,#3681,.T.);
#1796=ORIENTED_EDGE('',*,*,#3856,.F.);
#1797=ORIENTED_EDGE('',*,*,#3887,.F.);
#1798=ORIENTED_EDGE('',*,*,#3684,.F.);
#1799=ORIENTED_EDGE('',*,*,#3888,.T.);
#1800=ORIENTED_EDGE('',*,*,#3688,.F.);
#1801=ORIENTED_EDGE('',*,*,#3686,.F.);
#1802=ORIENTED_EDGE('',*,*,#3854,.F.);
#1803=ORIENTED_EDGE('',*,*,#3691,.T.);
#1804=ORIENTED_EDGE('',*,*,#3689,.F.);
#1805=ORIENTED_EDGE('',*,*,#3889,.F.);
#1806=ORIENTED_EDGE('',*,*,#3695,.F.);
#1807=ORIENTED_EDGE('',*,*,#3693,.T.);
#1808=ORIENTED_EDGE('',*,*,#3853,.F.);
#1809=ORIENTED_EDGE('',*,*,#3890,.F.);
#1810=ORIENTED_EDGE('',*,*,#3696,.F.);
#1811=ORIENTED_EDGE('',*,*,#3891,.T.);
#1812=ORIENTED_EDGE('',*,*,#3700,.F.);
#1813=ORIENTED_EDGE('',*,*,#3698,.F.);
#1814=ORIENTED_EDGE('',*,*,#3851,.F.);
#1815=ORIENTED_EDGE('',*,*,#3703,.T.);
#1816=ORIENTED_EDGE('',*,*,#3701,.F.);
#1817=ORIENTED_EDGE('',*,*,#3892,.F.);
#1818=ORIENTED_EDGE('',*,*,#3707,.F.);
#1819=ORIENTED_EDGE('',*,*,#3705,.T.);
#1820=ORIENTED_EDGE('',*,*,#3850,.F.);
#1821=ORIENTED_EDGE('',*,*,#3893,.F.);
#1822=ORIENTED_EDGE('',*,*,#3708,.F.);
#1823=ORIENTED_EDGE('',*,*,#3894,.T.);
#1824=ORIENTED_EDGE('',*,*,#3712,.F.);
#1825=ORIENTED_EDGE('',*,*,#3710,.F.);
#1826=ORIENTED_EDGE('',*,*,#3848,.F.);
#1827=ORIENTED_EDGE('',*,*,#3715,.T.);
#1828=ORIENTED_EDGE('',*,*,#3713,.F.);
#1829=ORIENTED_EDGE('',*,*,#3895,.F.);
#1830=ORIENTED_EDGE('',*,*,#3719,.F.);
#1831=ORIENTED_EDGE('',*,*,#3717,.T.);
#1832=ORIENTED_EDGE('',*,*,#3847,.F.);
#1833=ORIENTED_EDGE('',*,*,#3896,.F.);
#1834=ORIENTED_EDGE('',*,*,#3720,.F.);
#1835=ORIENTED_EDGE('',*,*,#3897,.T.);
#1836=ORIENTED_EDGE('',*,*,#3724,.F.);
#1837=ORIENTED_EDGE('',*,*,#3722,.F.);
#1838=ORIENTED_EDGE('',*,*,#3845,.F.);
#1839=ORIENTED_EDGE('',*,*,#3727,.T.);
#1840=ORIENTED_EDGE('',*,*,#3725,.F.);
#1841=ORIENTED_EDGE('',*,*,#3898,.F.);
#1842=ORIENTED_EDGE('',*,*,#3731,.F.);
#1843=ORIENTED_EDGE('',*,*,#3729,.T.);
#1844=ORIENTED_EDGE('',*,*,#3844,.F.);
#1845=ORIENTED_EDGE('',*,*,#3899,.F.);
#1846=ORIENTED_EDGE('',*,*,#3732,.F.);
#1847=ORIENTED_EDGE('',*,*,#3900,.T.);
#1848=ORIENTED_EDGE('',*,*,#3736,.F.);
#1849=ORIENTED_EDGE('',*,*,#3734,.F.);
#1850=ORIENTED_EDGE('',*,*,#3842,.F.);
#1851=ORIENTED_EDGE('',*,*,#3739,.T.);
#1852=ORIENTED_EDGE('',*,*,#3737,.F.);
#1853=ORIENTED_EDGE('',*,*,#3901,.F.);
#1854=ORIENTED_EDGE('',*,*,#3743,.F.);
#1855=ORIENTED_EDGE('',*,*,#3741,.T.);
#1856=ORIENTED_EDGE('',*,*,#3841,.F.);
#1857=ORIENTED_EDGE('',*,*,#3902,.F.);
#1858=ORIENTED_EDGE('',*,*,#3744,.F.);
#1859=ORIENTED_EDGE('',*,*,#3903,.T.);
#1860=ORIENTED_EDGE('',*,*,#3748,.F.);
#1861=ORIENTED_EDGE('',*,*,#3746,.F.);
#1862=ORIENTED_EDGE('',*,*,#3839,.F.);
#1863=ORIENTED_EDGE('',*,*,#3751,.T.);
#1864=ORIENTED_EDGE('',*,*,#3749,.F.);
#1865=ORIENTED_EDGE('',*,*,#3904,.F.);
#1866=ORIENTED_EDGE('',*,*,#3755,.F.);
#1867=ORIENTED_EDGE('',*,*,#3753,.T.);
#1868=ORIENTED_EDGE('',*,*,#3838,.F.);
#1869=ORIENTED_EDGE('',*,*,#3905,.F.);
#1870=ORIENTED_EDGE('',*,*,#3756,.F.);
#1871=ORIENTED_EDGE('',*,*,#3906,.T.);
#1872=ORIENTED_EDGE('',*,*,#3760,.F.);
#1873=ORIENTED_EDGE('',*,*,#3758,.F.);
#1874=ORIENTED_EDGE('',*,*,#3836,.F.);
#1875=ORIENTED_EDGE('',*,*,#3763,.T.);
#1876=ORIENTED_EDGE('',*,*,#3761,.F.);
#1877=ORIENTED_EDGE('',*,*,#3907,.F.);
#1878=ORIENTED_EDGE('',*,*,#3767,.F.);
#1879=ORIENTED_EDGE('',*,*,#3765,.T.);
#1880=ORIENTED_EDGE('',*,*,#3835,.F.);
#1881=ORIENTED_EDGE('',*,*,#3908,.F.);
#1882=ORIENTED_EDGE('',*,*,#3768,.F.);
#1883=ORIENTED_EDGE('',*,*,#3909,.T.);
#1884=ORIENTED_EDGE('',*,*,#3772,.F.);
#1885=ORIENTED_EDGE('',*,*,#3770,.F.);
#1886=ORIENTED_EDGE('',*,*,#3833,.F.);
#1887=ORIENTED_EDGE('',*,*,#3775,.T.);
#1888=ORIENTED_EDGE('',*,*,#3773,.F.);
#1889=ORIENTED_EDGE('',*,*,#3910,.F.);
#1890=ORIENTED_EDGE('',*,*,#3779,.F.);
#1891=ORIENTED_EDGE('',*,*,#3777,.T.);
#1892=ORIENTED_EDGE('',*,*,#3832,.F.);
#1893=ORIENTED_EDGE('',*,*,#3911,.F.);
#1894=ORIENTED_EDGE('',*,*,#3780,.F.);
#1895=ORIENTED_EDGE('',*,*,#3912,.T.);
#1896=ORIENTED_EDGE('',*,*,#3784,.F.);
#1897=ORIENTED_EDGE('',*,*,#3782,.F.);
#1898=ORIENTED_EDGE('',*,*,#3830,.F.);
#1899=ORIENTED_EDGE('',*,*,#3787,.T.);
#1900=ORIENTED_EDGE('',*,*,#3785,.F.);
#1901=ORIENTED_EDGE('',*,*,#3913,.F.);
#1902=ORIENTED_EDGE('',*,*,#3791,.F.);
#1903=ORIENTED_EDGE('',*,*,#3789,.T.);
#1904=ORIENTED_EDGE('',*,*,#3829,.F.);
#1905=ORIENTED_EDGE('',*,*,#3914,.F.);
#1906=ORIENTED_EDGE('',*,*,#3793,.T.);
#1907=ORIENTED_EDGE('',*,*,#3915,.T.);
#1908=ORIENTED_EDGE('',*,*,#3794,.F.);
#1909=ORIENTED_EDGE('',*,*,#3914,.T.);
#1910=ORIENTED_EDGE('',*,*,#3828,.F.);
#1911=ORIENTED_EDGE('',*,*,#3796,.T.);
#1912=ORIENTED_EDGE('',*,*,#3858,.F.);
#1913=ORIENTED_EDGE('',*,*,#3798,.T.);
#1914=ORIENTED_EDGE('',*,*,#3827,.F.);
#1915=ORIENTED_EDGE('',*,*,#3859,.T.);
#1916=ORIENTED_EDGE('',*,*,#3857,.F.);
#1917=ORIENTED_EDGE('',*,*,#3916,.F.);
#1918=ORIENTED_EDGE('',*,*,#3885,.F.);
#1919=ORIENTED_EDGE('',*,*,#3884,.T.);
#1920=ORIENTED_EDGE('',*,*,#3800,.F.);
#1921=ORIENTED_EDGE('',*,*,#3886,.T.);
#1922=ORIENTED_EDGE('',*,*,#3882,.F.);
#1923=ORIENTED_EDGE('',*,*,#3881,.T.);
#1924=ORIENTED_EDGE('',*,*,#3803,.F.);
#1925=ORIENTED_EDGE('',*,*,#3883,.T.);
#1926=ORIENTED_EDGE('',*,*,#3879,.F.);
#1927=ORIENTED_EDGE('',*,*,#3878,.T.);
#1928=ORIENTED_EDGE('',*,*,#3806,.F.);
#1929=ORIENTED_EDGE('',*,*,#3880,.T.);
#1930=ORIENTED_EDGE('',*,*,#3876,.F.);
#1931=ORIENTED_EDGE('',*,*,#3875,.T.);
#1932=ORIENTED_EDGE('',*,*,#3809,.F.);
#1933=ORIENTED_EDGE('',*,*,#3877,.T.);
#1934=ORIENTED_EDGE('',*,*,#3873,.F.);
#1935=ORIENTED_EDGE('',*,*,#3872,.T.);
#1936=ORIENTED_EDGE('',*,*,#3812,.F.);
#1937=ORIENTED_EDGE('',*,*,#3874,.T.);
#1938=ORIENTED_EDGE('',*,*,#3870,.F.);
#1939=ORIENTED_EDGE('',*,*,#3869,.T.);
#1940=ORIENTED_EDGE('',*,*,#3815,.F.);
#1941=ORIENTED_EDGE('',*,*,#3871,.T.);
#1942=ORIENTED_EDGE('',*,*,#3867,.F.);
#1943=ORIENTED_EDGE('',*,*,#3866,.T.);
#1944=ORIENTED_EDGE('',*,*,#3818,.F.);
#1945=ORIENTED_EDGE('',*,*,#3868,.T.);
#1946=ORIENTED_EDGE('',*,*,#3864,.F.);
#1947=ORIENTED_EDGE('',*,*,#3863,.T.);
#1948=ORIENTED_EDGE('',*,*,#3821,.F.);
#1949=ORIENTED_EDGE('',*,*,#3865,.T.);
#1950=ORIENTED_EDGE('',*,*,#3861,.F.);
#1951=ORIENTED_EDGE('',*,*,#3860,.T.);
#1952=ORIENTED_EDGE('',*,*,#3824,.F.);
#1953=ORIENTED_EDGE('',*,*,#3862,.T.);
#1954=ORIENTED_EDGE('',*,*,#3912,.F.);
#1955=ORIENTED_EDGE('',*,*,#3911,.T.);
#1956=ORIENTED_EDGE('',*,*,#3831,.F.);
#1957=ORIENTED_EDGE('',*,*,#3913,.T.);
#1958=ORIENTED_EDGE('',*,*,#3909,.F.);
#1959=ORIENTED_EDGE('',*,*,#3908,.T.);
#1960=ORIENTED_EDGE('',*,*,#3834,.F.);
#1961=ORIENTED_EDGE('',*,*,#3910,.T.);
#1962=ORIENTED_EDGE('',*,*,#3906,.F.);
#1963=ORIENTED_EDGE('',*,*,#3905,.T.);
#1964=ORIENTED_EDGE('',*,*,#3837,.F.);
#1965=ORIENTED_EDGE('',*,*,#3907,.T.);
#1966=ORIENTED_EDGE('',*,*,#3903,.F.);
#1967=ORIENTED_EDGE('',*,*,#3902,.T.);
#1968=ORIENTED_EDGE('',*,*,#3840,.F.);
#1969=ORIENTED_EDGE('',*,*,#3904,.T.);
#1970=ORIENTED_EDGE('',*,*,#3900,.F.);
#1971=ORIENTED_EDGE('',*,*,#3899,.T.);
#1972=ORIENTED_EDGE('',*,*,#3843,.F.);
#1973=ORIENTED_EDGE('',*,*,#3901,.T.);
#1974=ORIENTED_EDGE('',*,*,#3897,.F.);
#1975=ORIENTED_EDGE('',*,*,#3896,.T.);
#1976=ORIENTED_EDGE('',*,*,#3846,.F.);
#1977=ORIENTED_EDGE('',*,*,#3898,.T.);
#1978=ORIENTED_EDGE('',*,*,#3894,.F.);
#1979=ORIENTED_EDGE('',*,*,#3893,.T.);
#1980=ORIENTED_EDGE('',*,*,#3849,.F.);
#1981=ORIENTED_EDGE('',*,*,#3895,.T.);
#1982=ORIENTED_EDGE('',*,*,#3891,.F.);
#1983=ORIENTED_EDGE('',*,*,#3890,.T.);
#1984=ORIENTED_EDGE('',*,*,#3852,.F.);
#1985=ORIENTED_EDGE('',*,*,#3892,.T.);
#1986=ORIENTED_EDGE('',*,*,#3888,.F.);
#1987=ORIENTED_EDGE('',*,*,#3887,.T.);
#1988=ORIENTED_EDGE('',*,*,#3855,.F.);
#1989=ORIENTED_EDGE('',*,*,#3889,.T.);
#1990=ORIENTED_EDGE('',*,*,#3915,.F.);
#1991=ORIENTED_EDGE('',*,*,#3917,.F.);
#1992=ORIENTED_EDGE('',*,*,#3916,.T.);
#1993=ORIENTED_EDGE('',*,*,#3917,.T.);
#1994=ORIENTED_EDGE('',*,*,#3918,.F.);
#1995=ORIENTED_EDGE('',*,*,#3919,.F.);
#1996=ORIENTED_EDGE('',*,*,#3920,.F.);
#1997=ORIENTED_EDGE('',*,*,#3918,.T.);
#1998=ORIENTED_EDGE('',*,*,#3921,.F.);
#1999=ORIENTED_EDGE('',*,*,#3919,.T.);
#2000=ORIENTED_EDGE('',*,*,#3922,.T.);
#2001=ORIENTED_EDGE('',*,*,#3923,.T.);
#2002=ORIENTED_EDGE('',*,*,#3920,.T.);
#2003=ORIENTED_EDGE('',*,*,#3921,.T.);
#2004=ORIENTED_EDGE('',*,*,#3924,.T.);
#2005=ORIENTED_EDGE('',*,*,#3922,.F.);
#2006=ORIENTED_EDGE('',*,*,#3923,.F.);
#2007=ORIENTED_EDGE('',*,*,#3925,.T.);
#2008=ORIENTED_EDGE('',*,*,#3926,.T.);
#2009=ORIENTED_EDGE('',*,*,#3926,.F.);
#2010=ORIENTED_EDGE('',*,*,#3925,.F.);
#2011=ORIENTED_EDGE('',*,*,#3927,.T.);
#2012=ORIENTED_EDGE('',*,*,#3928,.T.);
#2013=ORIENTED_EDGE('',*,*,#3924,.F.);
#2014=ORIENTED_EDGE('',*,*,#3929,.F.);
#2015=ORIENTED_EDGE('',*,*,#3928,.F.);
#2016=ORIENTED_EDGE('',*,*,#3927,.F.);
#2017=ORIENTED_EDGE('',*,*,#3930,.T.);
#2018=ORIENTED_EDGE('',*,*,#3931,.T.);
#2019=ORIENTED_EDGE('',*,*,#3932,.F.);
#2020=ORIENTED_EDGE('',*,*,#3933,.F.);
#2021=ORIENTED_EDGE('',*,*,#3929,.T.);
#2022=ORIENTED_EDGE('',*,*,#3934,.F.);
#2023=ORIENTED_EDGE('',*,*,#3935,.F.);
#2024=ORIENTED_EDGE('',*,*,#3936,.F.);
#2025=ORIENTED_EDGE('',*,*,#3930,.F.);
#2026=ORIENTED_EDGE('',*,*,#3931,.F.);
#2027=ORIENTED_EDGE('',*,*,#3936,.T.);
#2028=ORIENTED_EDGE('',*,*,#3937,.F.);
#2029=ORIENTED_EDGE('',*,*,#3934,.T.);
#2030=ORIENTED_EDGE('',*,*,#3938,.T.);
#2031=ORIENTED_EDGE('',*,*,#3939,.T.);
#2032=ORIENTED_EDGE('',*,*,#3932,.T.);
#2033=ORIENTED_EDGE('',*,*,#3933,.T.);
#2034=ORIENTED_EDGE('',*,*,#3940,.T.);
#2035=ORIENTED_EDGE('',*,*,#3941,.T.);
#2036=ORIENTED_EDGE('',*,*,#3935,.T.);
#2037=ORIENTED_EDGE('',*,*,#3937,.T.);
#2038=ORIENTED_EDGE('',*,*,#3939,.F.);
#2039=ORIENTED_EDGE('',*,*,#3942,.T.);
#2040=ORIENTED_EDGE('',*,*,#3943,.T.);
#2041=ORIENTED_EDGE('',*,*,#3944,.T.);
#2042=ORIENTED_EDGE('',*,*,#3942,.F.);
#2043=ORIENTED_EDGE('',*,*,#3938,.F.);
#2044=ORIENTED_EDGE('',*,*,#3944,.F.);
#2045=ORIENTED_EDGE('',*,*,#3945,.T.);
#2046=ORIENTED_EDGE('',*,*,#3946,.T.);
#2047=ORIENTED_EDGE('',*,*,#3947,.T.);
#2048=ORIENTED_EDGE('',*,*,#3948,.T.);
#2049=ORIENTED_EDGE('',*,*,#3941,.F.);
#2050=ORIENTED_EDGE('',*,*,#3949,.T.);
#2051=ORIENTED_EDGE('',*,*,#3946,.F.);
#2052=ORIENTED_EDGE('',*,*,#3940,.F.);
#2053=ORIENTED_EDGE('',*,*,#3948,.F.);
#2054=ORIENTED_EDGE('',*,*,#3947,.F.);
#2055=ORIENTED_EDGE('',*,*,#3949,.F.);
#2056=ORIENTED_EDGE('',*,*,#3943,.F.);
#2057=ORIENTED_EDGE('',*,*,#3945,.F.);
#2058=ORIENTED_EDGE('',*,*,#3950,.F.);
#2059=ORIENTED_EDGE('',*,*,#3951,.F.);
#2060=ORIENTED_EDGE('',*,*,#3952,.F.);
#2061=ORIENTED_EDGE('',*,*,#3950,.T.);
#2062=ORIENTED_EDGE('',*,*,#3953,.F.);
#2063=ORIENTED_EDGE('',*,*,#3951,.T.);
#2064=ORIENTED_EDGE('',*,*,#3954,.T.);
#2065=ORIENTED_EDGE('',*,*,#3955,.T.);
#2066=ORIENTED_EDGE('',*,*,#3952,.T.);
#2067=ORIENTED_EDGE('',*,*,#3953,.T.);
#2068=ORIENTED_EDGE('',*,*,#3956,.T.);
#2069=ORIENTED_EDGE('',*,*,#3954,.F.);
#2070=ORIENTED_EDGE('',*,*,#3955,.F.);
#2071=ORIENTED_EDGE('',*,*,#3957,.T.);
#2072=ORIENTED_EDGE('',*,*,#3958,.T.);
#2073=ORIENTED_EDGE('',*,*,#3958,.F.);
#2074=ORIENTED_EDGE('',*,*,#3957,.F.);
#2075=ORIENTED_EDGE('',*,*,#3959,.T.);
#2076=ORIENTED_EDGE('',*,*,#3960,.T.);
#2077=ORIENTED_EDGE('',*,*,#3956,.F.);
#2078=ORIENTED_EDGE('',*,*,#3961,.F.);
#2079=ORIENTED_EDGE('',*,*,#3960,.F.);
#2080=ORIENTED_EDGE('',*,*,#3959,.F.);
#2081=ORIENTED_EDGE('',*,*,#3962,.T.);
#2082=ORIENTED_EDGE('',*,*,#3963,.T.);
#2083=ORIENTED_EDGE('',*,*,#3964,.F.);
#2084=ORIENTED_EDGE('',*,*,#3965,.F.);
#2085=ORIENTED_EDGE('',*,*,#3961,.T.);
#2086=ORIENTED_EDGE('',*,*,#3966,.F.);
#2087=ORIENTED_EDGE('',*,*,#3967,.F.);
#2088=ORIENTED_EDGE('',*,*,#3968,.F.);
#2089=ORIENTED_EDGE('',*,*,#3962,.F.);
#2090=ORIENTED_EDGE('',*,*,#3963,.F.);
#2091=ORIENTED_EDGE('',*,*,#3968,.T.);
#2092=ORIENTED_EDGE('',*,*,#3969,.F.);
#2093=ORIENTED_EDGE('',*,*,#3966,.T.);
#2094=ORIENTED_EDGE('',*,*,#3970,.T.);
#2095=ORIENTED_EDGE('',*,*,#3971,.T.);
#2096=ORIENTED_EDGE('',*,*,#3964,.T.);
#2097=ORIENTED_EDGE('',*,*,#3965,.T.);
#2098=ORIENTED_EDGE('',*,*,#3972,.T.);
#2099=ORIENTED_EDGE('',*,*,#3973,.T.);
#2100=ORIENTED_EDGE('',*,*,#3967,.T.);
#2101=ORIENTED_EDGE('',*,*,#3969,.T.);
#2102=ORIENTED_EDGE('',*,*,#3971,.F.);
#2103=ORIENTED_EDGE('',*,*,#3974,.T.);
#2104=ORIENTED_EDGE('',*,*,#3975,.T.);
#2105=ORIENTED_EDGE('',*,*,#3976,.T.);
#2106=ORIENTED_EDGE('',*,*,#3974,.F.);
#2107=ORIENTED_EDGE('',*,*,#3970,.F.);
#2108=ORIENTED_EDGE('',*,*,#3976,.F.);
#2109=ORIENTED_EDGE('',*,*,#3977,.T.);
#2110=ORIENTED_EDGE('',*,*,#3978,.T.);
#2111=ORIENTED_EDGE('',*,*,#3979,.T.);
#2112=ORIENTED_EDGE('',*,*,#3980,.T.);
#2113=ORIENTED_EDGE('',*,*,#3973,.F.);
#2114=ORIENTED_EDGE('',*,*,#3981,.T.);
#2115=ORIENTED_EDGE('',*,*,#3978,.F.);
#2116=ORIENTED_EDGE('',*,*,#3972,.F.);
#2117=ORIENTED_EDGE('',*,*,#3980,.F.);
#2118=ORIENTED_EDGE('',*,*,#3979,.F.);
#2119=ORIENTED_EDGE('',*,*,#3981,.F.);
#2120=ORIENTED_EDGE('',*,*,#3975,.F.);
#2121=ORIENTED_EDGE('',*,*,#3977,.F.);
#2122=ORIENTED_EDGE('',*,*,#3982,.T.);
#2123=ORIENTED_EDGE('',*,*,#3983,.T.);
#2124=ORIENTED_EDGE('',*,*,#3984,.T.);
#2125=ORIENTED_EDGE('',*,*,#3984,.F.);
#2126=ORIENTED_EDGE('',*,*,#3985,.T.);
#2127=ORIENTED_EDGE('',*,*,#3986,.T.);
#2128=ORIENTED_EDGE('',*,*,#3987,.T.);
#2129=ORIENTED_EDGE('',*,*,#3983,.F.);
#2130=ORIENTED_EDGE('',*,*,#3982,.F.);
#2131=ORIENTED_EDGE('',*,*,#3985,.F.);
#2132=ORIENTED_EDGE('',*,*,#3988,.F.);
#2133=ORIENTED_EDGE('',*,*,#3989,.F.);
#2134=ORIENTED_EDGE('',*,*,#3990,.T.);
#2135=ORIENTED_EDGE('',*,*,#3987,.F.);
#2136=ORIENTED_EDGE('',*,*,#3986,.F.);
#2137=ORIENTED_EDGE('',*,*,#3991,.T.);
#2138=ORIENTED_EDGE('',*,*,#3992,.T.);
#2139=ORIENTED_EDGE('',*,*,#3993,.T.);
#2140=ORIENTED_EDGE('',*,*,#3988,.T.);
#2141=ORIENTED_EDGE('',*,*,#3994,.T.);
#2142=ORIENTED_EDGE('',*,*,#3991,.F.);
#2143=ORIENTED_EDGE('',*,*,#3989,.T.);
#2144=ORIENTED_EDGE('',*,*,#3993,.F.);
#2145=ORIENTED_EDGE('',*,*,#3990,.F.);
#2146=ORIENTED_EDGE('',*,*,#3995,.T.);
#2147=ORIENTED_EDGE('',*,*,#3994,.F.);
#2148=ORIENTED_EDGE('',*,*,#3992,.F.);
#2149=ORIENTED_EDGE('',*,*,#3996,.T.);
#2150=ORIENTED_EDGE('',*,*,#3997,.F.);
#2151=ORIENTED_EDGE('',*,*,#3998,.F.);
#2152=ORIENTED_EDGE('',*,*,#3995,.F.);
#2153=ORIENTED_EDGE('',*,*,#3996,.F.);
#2154=ORIENTED_EDGE('',*,*,#3999,.T.);
#2155=ORIENTED_EDGE('',*,*,#4000,.T.);
#2156=ORIENTED_EDGE('',*,*,#4001,.T.);
#2157=ORIENTED_EDGE('',*,*,#3997,.T.);
#2158=ORIENTED_EDGE('',*,*,#4002,.T.);
#2159=ORIENTED_EDGE('',*,*,#4003,.T.);
#2160=ORIENTED_EDGE('',*,*,#3998,.T.);
#2161=ORIENTED_EDGE('',*,*,#4001,.F.);
#2162=ORIENTED_EDGE('',*,*,#4004,.T.);
#2163=ORIENTED_EDGE('',*,*,#4002,.F.);
#2164=ORIENTED_EDGE('',*,*,#4005,.T.);
#2165=ORIENTED_EDGE('',*,*,#4000,.F.);
#2166=ORIENTED_EDGE('',*,*,#4006,.T.);
#2167=ORIENTED_EDGE('',*,*,#4007,.T.);
#2168=ORIENTED_EDGE('',*,*,#3999,.F.);
#2169=ORIENTED_EDGE('',*,*,#4005,.F.);
#2170=ORIENTED_EDGE('',*,*,#4008,.T.);
#2171=ORIENTED_EDGE('',*,*,#4006,.F.);
#2172=ORIENTED_EDGE('',*,*,#4009,.T.);
#2173=ORIENTED_EDGE('',*,*,#4003,.F.);
#2174=ORIENTED_EDGE('',*,*,#4004,.F.);
#2175=ORIENTED_EDGE('',*,*,#4007,.F.);
#2176=ORIENTED_EDGE('',*,*,#4008,.F.);
#2177=ORIENTED_EDGE('',*,*,#4010,.F.);
#2178=ORIENTED_EDGE('',*,*,#4011,.F.);
#2179=ORIENTED_EDGE('',*,*,#4009,.F.);
#2180=ORIENTED_EDGE('',*,*,#4012,.T.);
#2181=ORIENTED_EDGE('',*,*,#4013,.T.);
#2182=ORIENTED_EDGE('',*,*,#4014,.T.);
#2183=ORIENTED_EDGE('',*,*,#4010,.T.);
#2184=ORIENTED_EDGE('',*,*,#4015,.T.);
#2185=ORIENTED_EDGE('',*,*,#4013,.F.);
#2186=ORIENTED_EDGE('',*,*,#4011,.T.);
#2187=ORIENTED_EDGE('',*,*,#4014,.F.);
#2188=ORIENTED_EDGE('',*,*,#4012,.F.);
#2189=ORIENTED_EDGE('',*,*,#4015,.F.);
#2190=ORIENTED_EDGE('',*,*,#4016,.T.);
#2191=ORIENTED_EDGE('',*,*,#4017,.T.);
#2192=ORIENTED_EDGE('',*,*,#4018,.T.);
#2193=ORIENTED_EDGE('',*,*,#4018,.F.);
#2194=ORIENTED_EDGE('',*,*,#4019,.T.);
#2195=ORIENTED_EDGE('',*,*,#4020,.T.);
#2196=ORIENTED_EDGE('',*,*,#4021,.T.);
#2197=ORIENTED_EDGE('',*,*,#4017,.F.);
#2198=ORIENTED_EDGE('',*,*,#4016,.F.);
#2199=ORIENTED_EDGE('',*,*,#4019,.F.);
#2200=ORIENTED_EDGE('',*,*,#4022,.F.);
#2201=ORIENTED_EDGE('',*,*,#4023,.F.);
#2202=ORIENTED_EDGE('',*,*,#4024,.T.);
#2203=ORIENTED_EDGE('',*,*,#4021,.F.);
#2204=ORIENTED_EDGE('',*,*,#4020,.F.);
#2205=ORIENTED_EDGE('',*,*,#4025,.T.);
#2206=ORIENTED_EDGE('',*,*,#4026,.T.);
#2207=ORIENTED_EDGE('',*,*,#4027,.T.);
#2208=ORIENTED_EDGE('',*,*,#4022,.T.);
#2209=ORIENTED_EDGE('',*,*,#4028,.T.);
#2210=ORIENTED_EDGE('',*,*,#4025,.F.);
#2211=ORIENTED_EDGE('',*,*,#4023,.T.);
#2212=ORIENTED_EDGE('',*,*,#4027,.F.);
#2213=ORIENTED_EDGE('',*,*,#4024,.F.);
#2214=ORIENTED_EDGE('',*,*,#4029,.T.);
#2215=ORIENTED_EDGE('',*,*,#4028,.F.);
#2216=ORIENTED_EDGE('',*,*,#4026,.F.);
#2217=ORIENTED_EDGE('',*,*,#4030,.T.);
#2218=ORIENTED_EDGE('',*,*,#4031,.F.);
#2219=ORIENTED_EDGE('',*,*,#4032,.F.);
#2220=ORIENTED_EDGE('',*,*,#4029,.F.);
#2221=ORIENTED_EDGE('',*,*,#4030,.F.);
#2222=ORIENTED_EDGE('',*,*,#4033,.T.);
#2223=ORIENTED_EDGE('',*,*,#4034,.T.);
#2224=ORIENTED_EDGE('',*,*,#4035,.T.);
#2225=ORIENTED_EDGE('',*,*,#4031,.T.);
#2226=ORIENTED_EDGE('',*,*,#4036,.T.);
#2227=ORIENTED_EDGE('',*,*,#4037,.T.);
#2228=ORIENTED_EDGE('',*,*,#4032,.T.);
#2229=ORIENTED_EDGE('',*,*,#4035,.F.);
#2230=ORIENTED_EDGE('',*,*,#4038,.T.);
#2231=ORIENTED_EDGE('',*,*,#4036,.F.);
#2232=ORIENTED_EDGE('',*,*,#4039,.T.);
#2233=ORIENTED_EDGE('',*,*,#4034,.F.);
#2234=ORIENTED_EDGE('',*,*,#4040,.T.);
#2235=ORIENTED_EDGE('',*,*,#4041,.T.);
#2236=ORIENTED_EDGE('',*,*,#4033,.F.);
#2237=ORIENTED_EDGE('',*,*,#4039,.F.);
#2238=ORIENTED_EDGE('',*,*,#4042,.T.);
#2239=ORIENTED_EDGE('',*,*,#4040,.F.);
#2240=ORIENTED_EDGE('',*,*,#4043,.T.);
#2241=ORIENTED_EDGE('',*,*,#4037,.F.);
#2242=ORIENTED_EDGE('',*,*,#4038,.F.);
#2243=ORIENTED_EDGE('',*,*,#4041,.F.);
#2244=ORIENTED_EDGE('',*,*,#4042,.F.);
#2245=ORIENTED_EDGE('',*,*,#4044,.F.);
#2246=ORIENTED_EDGE('',*,*,#4045,.F.);
#2247=ORIENTED_EDGE('',*,*,#4043,.F.);
#2248=ORIENTED_EDGE('',*,*,#4046,.T.);
#2249=ORIENTED_EDGE('',*,*,#4047,.T.);
#2250=ORIENTED_EDGE('',*,*,#4048,.T.);
#2251=ORIENTED_EDGE('',*,*,#4044,.T.);
#2252=ORIENTED_EDGE('',*,*,#4049,.T.);
#2253=ORIENTED_EDGE('',*,*,#4047,.F.);
#2254=ORIENTED_EDGE('',*,*,#4045,.T.);
#2255=ORIENTED_EDGE('',*,*,#4048,.F.);
#2256=ORIENTED_EDGE('',*,*,#4046,.F.);
#2257=ORIENTED_EDGE('',*,*,#4049,.F.);
#2258=ORIENTED_EDGE('',*,*,#4050,.F.);
#2259=ORIENTED_EDGE('',*,*,#4051,.F.);
#2260=ORIENTED_EDGE('',*,*,#4052,.T.);
#2261=ORIENTED_EDGE('',*,*,#4050,.T.);
#2262=ORIENTED_EDGE('',*,*,#4053,.T.);
#2263=ORIENTED_EDGE('',*,*,#4051,.T.);
#2264=ORIENTED_EDGE('',*,*,#4052,.F.);
#2265=ORIENTED_EDGE('',*,*,#4054,.F.);
#2266=ORIENTED_EDGE('',*,*,#4055,.F.);
#2267=ORIENTED_EDGE('',*,*,#4053,.F.);
#2268=ORIENTED_EDGE('',*,*,#4054,.T.);
#2269=ORIENTED_EDGE('',*,*,#4056,.T.);
#2270=ORIENTED_EDGE('',*,*,#4055,.T.);
#2271=ORIENTED_EDGE('',*,*,#4057,.T.);
#2272=ORIENTED_EDGE('',*,*,#4056,.F.);
#2273=ORIENTED_EDGE('',*,*,#4058,.F.);
#2274=ORIENTED_EDGE('',*,*,#4059,.F.);
#2275=ORIENTED_EDGE('',*,*,#4057,.F.);
#2276=ORIENTED_EDGE('',*,*,#4060,.T.);
#2277=ORIENTED_EDGE('',*,*,#4058,.T.);
#2278=ORIENTED_EDGE('',*,*,#4061,.T.);
#2279=ORIENTED_EDGE('',*,*,#4059,.T.);
#2280=ORIENTED_EDGE('',*,*,#4060,.F.);
#2281=ORIENTED_EDGE('',*,*,#4062,.F.);
#2282=ORIENTED_EDGE('',*,*,#4063,.F.);
#2283=ORIENTED_EDGE('',*,*,#4061,.F.);
#2284=ORIENTED_EDGE('',*,*,#4062,.T.);
#2285=ORIENTED_EDGE('',*,*,#4064,.T.);
#2286=ORIENTED_EDGE('',*,*,#4063,.T.);
#2287=ORIENTED_EDGE('',*,*,#4065,.T.);
#2288=ORIENTED_EDGE('',*,*,#4066,.F.);
#2289=ORIENTED_EDGE('',*,*,#4064,.F.);
#2290=ORIENTED_EDGE('',*,*,#4067,.F.);
#2291=ORIENTED_EDGE('',*,*,#4065,.F.);
#2292=ORIENTED_EDGE('',*,*,#4068,.T.);
#2293=ORIENTED_EDGE('',*,*,#4066,.T.);
#2294=ORIENTED_EDGE('',*,*,#4069,.T.);
#2295=ORIENTED_EDGE('',*,*,#4067,.T.);
#2296=ORIENTED_EDGE('',*,*,#4068,.F.);
#2297=ORIENTED_EDGE('',*,*,#4070,.F.);
#2298=ORIENTED_EDGE('',*,*,#4069,.F.);
#2299=ORIENTED_EDGE('',*,*,#4071,.F.);
#2300=ORIENTED_EDGE('',*,*,#4070,.T.);
#2301=ORIENTED_EDGE('',*,*,#4072,.T.);
#2302=ORIENTED_EDGE('',*,*,#4071,.T.);
#2303=ORIENTED_EDGE('',*,*,#4073,.T.);
#2304=ORIENTED_EDGE('',*,*,#4074,.F.);
#2305=ORIENTED_EDGE('',*,*,#4072,.F.);
#2306=ORIENTED_EDGE('',*,*,#4075,.F.);
#2307=ORIENTED_EDGE('',*,*,#4073,.F.);
#2308=ORIENTED_EDGE('',*,*,#4076,.T.);
#2309=ORIENTED_EDGE('',*,*,#4074,.T.);
#2310=ORIENTED_EDGE('',*,*,#4075,.T.);
#2311=ORIENTED_EDGE('',*,*,#4077,.T.);
#2312=ORIENTED_EDGE('',*,*,#4078,.F.);
#2313=ORIENTED_EDGE('',*,*,#4076,.F.);
#2314=ORIENTED_EDGE('',*,*,#4077,.F.);
#2315=ORIENTED_EDGE('',*,*,#4079,.F.);
#2316=ORIENTED_EDGE('',*,*,#4080,.F.);
#2317=ORIENTED_EDGE('',*,*,#4078,.T.);
#2318=ORIENTED_EDGE('',*,*,#4079,.T.);
#2319=ORIENTED_EDGE('',*,*,#4081,.T.);
#2320=ORIENTED_EDGE('',*,*,#4080,.T.);
#2321=ORIENTED_EDGE('',*,*,#4082,.T.);
#2322=ORIENTED_EDGE('',*,*,#4081,.F.);
#2323=ORIENTED_EDGE('',*,*,#4083,.F.);
#2324=ORIENTED_EDGE('',*,*,#4084,.F.);
#2325=ORIENTED_EDGE('',*,*,#4085,.F.);
#2326=ORIENTED_EDGE('',*,*,#4086,.F.);
#2327=ORIENTED_EDGE('',*,*,#4087,.F.);
#2328=ORIENTED_EDGE('',*,*,#4088,.F.);
#2329=ORIENTED_EDGE('',*,*,#4089,.F.);
#2330=ORIENTED_EDGE('',*,*,#4090,.F.);
#2331=ORIENTED_EDGE('',*,*,#4091,.F.);
#2332=ORIENTED_EDGE('',*,*,#4092,.F.);
#2333=ORIENTED_EDGE('',*,*,#4093,.F.);
#2334=ORIENTED_EDGE('',*,*,#4094,.F.);
#2335=ORIENTED_EDGE('',*,*,#4095,.F.);
#2336=ORIENTED_EDGE('',*,*,#4096,.F.);
#2337=ORIENTED_EDGE('',*,*,#4097,.F.);
#2338=ORIENTED_EDGE('',*,*,#4098,.F.);
#2339=ORIENTED_EDGE('',*,*,#4099,.F.);
#2340=ORIENTED_EDGE('',*,*,#4100,.F.);
#2341=ORIENTED_EDGE('',*,*,#4101,.F.);
#2342=ORIENTED_EDGE('',*,*,#4102,.F.);
#2343=ORIENTED_EDGE('',*,*,#4082,.F.);
#2344=ORIENTED_EDGE('',*,*,#4103,.F.);
#2345=ORIENTED_EDGE('',*,*,#4083,.T.);
#2346=ORIENTED_EDGE('',*,*,#4104,.F.);
#2347=ORIENTED_EDGE('',*,*,#4102,.T.);
#2348=ORIENTED_EDGE('',*,*,#4101,.T.);
#2349=ORIENTED_EDGE('',*,*,#4105,.F.);
#2350=ORIENTED_EDGE('',*,*,#4106,.F.);
#2351=ORIENTED_EDGE('',*,*,#4100,.T.);
#2352=ORIENTED_EDGE('',*,*,#4107,.F.);
#2353=ORIENTED_EDGE('',*,*,#4099,.T.);
#2354=ORIENTED_EDGE('',*,*,#4108,.F.);
#2355=ORIENTED_EDGE('',*,*,#4098,.T.);
#2356=ORIENTED_EDGE('',*,*,#4109,.F.);
#2357=ORIENTED_EDGE('',*,*,#4097,.T.);
#2358=ORIENTED_EDGE('',*,*,#4110,.F.);
#2359=ORIENTED_EDGE('',*,*,#4096,.T.);
#2360=ORIENTED_EDGE('',*,*,#4111,.F.);
#2361=ORIENTED_EDGE('',*,*,#4095,.T.);
#2362=ORIENTED_EDGE('',*,*,#4112,.F.);
#2363=ORIENTED_EDGE('',*,*,#4094,.T.);
#2364=ORIENTED_EDGE('',*,*,#4113,.F.);
#2365=ORIENTED_EDGE('',*,*,#4093,.T.);
#2366=ORIENTED_EDGE('',*,*,#4114,.F.);
#2367=ORIENTED_EDGE('',*,*,#4092,.T.);
#2368=ORIENTED_EDGE('',*,*,#4115,.F.);
#2369=ORIENTED_EDGE('',*,*,#4091,.T.);
#2370=ORIENTED_EDGE('',*,*,#4116,.F.);
#2371=ORIENTED_EDGE('',*,*,#4090,.T.);
#2372=ORIENTED_EDGE('',*,*,#4117,.F.);
#2373=ORIENTED_EDGE('',*,*,#4089,.T.);
#2374=ORIENTED_EDGE('',*,*,#4118,.F.);
#2375=ORIENTED_EDGE('',*,*,#4088,.T.);
#2376=ORIENTED_EDGE('',*,*,#4119,.F.);
#2377=ORIENTED_EDGE('',*,*,#4087,.T.);
#2378=ORIENTED_EDGE('',*,*,#4120,.F.);
#2379=ORIENTED_EDGE('',*,*,#4086,.T.);
#2380=ORIENTED_EDGE('',*,*,#4121,.F.);
#2381=ORIENTED_EDGE('',*,*,#4085,.T.);
#2382=ORIENTED_EDGE('',*,*,#4122,.T.);
#2383=ORIENTED_EDGE('',*,*,#4123,.T.);
#2384=ORIENTED_EDGE('',*,*,#4084,.T.);
#2385=ORIENTED_EDGE('',*,*,#4103,.T.);
#2386=ORIENTED_EDGE('',*,*,#4124,.F.);
#2387=ORIENTED_EDGE('',*,*,#4125,.F.);
#2388=ORIENTED_EDGE('',*,*,#4126,.F.);
#2389=ORIENTED_EDGE('',*,*,#4121,.T.);
#2390=ORIENTED_EDGE('',*,*,#4120,.T.);
#2391=ORIENTED_EDGE('',*,*,#4119,.T.);
#2392=ORIENTED_EDGE('',*,*,#4118,.T.);
#2393=ORIENTED_EDGE('',*,*,#4117,.T.);
#2394=ORIENTED_EDGE('',*,*,#4116,.T.);
#2395=ORIENTED_EDGE('',*,*,#4115,.T.);
#2396=ORIENTED_EDGE('',*,*,#4114,.T.);
#2397=ORIENTED_EDGE('',*,*,#4113,.T.);
#2398=ORIENTED_EDGE('',*,*,#4112,.T.);
#2399=ORIENTED_EDGE('',*,*,#4111,.T.);
#2400=ORIENTED_EDGE('',*,*,#4110,.T.);
#2401=ORIENTED_EDGE('',*,*,#4109,.T.);
#2402=ORIENTED_EDGE('',*,*,#4108,.T.);
#2403=ORIENTED_EDGE('',*,*,#4107,.T.);
#2404=ORIENTED_EDGE('',*,*,#4106,.T.);
#2405=ORIENTED_EDGE('',*,*,#4105,.T.);
#2406=ORIENTED_EDGE('',*,*,#4104,.T.);
#2407=ORIENTED_EDGE('',*,*,#4127,.F.);
#2408=ORIENTED_EDGE('',*,*,#4122,.F.);
#2409=ORIENTED_EDGE('',*,*,#4123,.F.);
#2410=ORIENTED_EDGE('',*,*,#4128,.T.);
#2411=ORIENTED_EDGE('',*,*,#4129,.T.);
#2412=ORIENTED_EDGE('',*,*,#4124,.T.);
#2413=ORIENTED_EDGE('',*,*,#4125,.T.);
#2414=ORIENTED_EDGE('',*,*,#4130,.F.);
#2415=ORIENTED_EDGE('',*,*,#4131,.F.);
#2416=ORIENTED_EDGE('',*,*,#4127,.T.);
#2417=ORIENTED_EDGE('',*,*,#4132,.T.);
#2418=ORIENTED_EDGE('',*,*,#4133,.T.);
#2419=ORIENTED_EDGE('',*,*,#4129,.F.);
#2420=ORIENTED_EDGE('',*,*,#4128,.F.);
#2421=ORIENTED_EDGE('',*,*,#4126,.T.);
#2422=ORIENTED_EDGE('',*,*,#4130,.T.);
#2423=ORIENTED_EDGE('',*,*,#4131,.T.);
#2424=ORIENTED_EDGE('',*,*,#4134,.F.);
#2425=ORIENTED_EDGE('',*,*,#4135,.T.);
#2426=ORIENTED_EDGE('',*,*,#4136,.T.);
#2427=ORIENTED_EDGE('',*,*,#4132,.F.);
#2428=ORIENTED_EDGE('',*,*,#4133,.F.);
#2429=ORIENTED_EDGE('',*,*,#4137,.T.);
#2430=ORIENTED_EDGE('',*,*,#4134,.T.);
#2431=ORIENTED_EDGE('',*,*,#4136,.F.);
#2432=ORIENTED_EDGE('',*,*,#4138,.F.);
#2433=ORIENTED_EDGE('',*,*,#4139,.F.);
#2434=ORIENTED_EDGE('',*,*,#4140,.F.);
#2435=ORIENTED_EDGE('',*,*,#4140,.T.);
#2436=ORIENTED_EDGE('',*,*,#4141,.F.);
#2437=ORIENTED_EDGE('',*,*,#4138,.T.);
#2438=ORIENTED_EDGE('',*,*,#4135,.F.);
#2439=ORIENTED_EDGE('',*,*,#4142,.F.);
#2440=ORIENTED_EDGE('',*,*,#4143,.F.);
#2441=ORIENTED_EDGE('',*,*,#4137,.F.);
#2442=ORIENTED_EDGE('',*,*,#4141,.T.);
#2443=ORIENTED_EDGE('',*,*,#4139,.T.);
#2444=ORIENTED_EDGE('',*,*,#4144,.T.);
#2445=ORIENTED_EDGE('',*,*,#4145,.T.);
#2446=ORIENTED_EDGE('',*,*,#4146,.T.);
#2447=ORIENTED_EDGE('',*,*,#4147,.T.);
#2448=ORIENTED_EDGE('',*,*,#4148,.T.);
#2449=ORIENTED_EDGE('',*,*,#4149,.T.);
#2450=ORIENTED_EDGE('',*,*,#4150,.T.);
#2451=ORIENTED_EDGE('',*,*,#4151,.T.);
#2452=ORIENTED_EDGE('',*,*,#4152,.T.);
#2453=ORIENTED_EDGE('',*,*,#4153,.T.);
#2454=ORIENTED_EDGE('',*,*,#4154,.T.);
#2455=ORIENTED_EDGE('',*,*,#4155,.T.);
#2456=ORIENTED_EDGE('',*,*,#4156,.T.);
#2457=ORIENTED_EDGE('',*,*,#4157,.T.);
#2458=ORIENTED_EDGE('',*,*,#4158,.T.);
#2459=ORIENTED_EDGE('',*,*,#4159,.T.);
#2460=ORIENTED_EDGE('',*,*,#4160,.T.);
#2461=ORIENTED_EDGE('',*,*,#4161,.T.);
#2462=ORIENTED_EDGE('',*,*,#4162,.T.);
#2463=ORIENTED_EDGE('',*,*,#4163,.T.);
#2464=ORIENTED_EDGE('',*,*,#4164,.T.);
#2465=ORIENTED_EDGE('',*,*,#4165,.T.);
#2466=ORIENTED_EDGE('',*,*,#4166,.T.);
#2467=ORIENTED_EDGE('',*,*,#4167,.T.);
#2468=ORIENTED_EDGE('',*,*,#4168,.T.);
#2469=ORIENTED_EDGE('',*,*,#4169,.T.);
#2470=ORIENTED_EDGE('',*,*,#4143,.T.);
#2471=ORIENTED_EDGE('',*,*,#4142,.T.);
#2472=ORIENTED_EDGE('',*,*,#4170,.T.);
#2473=ORIENTED_EDGE('',*,*,#4171,.F.);
#2474=ORIENTED_EDGE('',*,*,#4172,.F.);
#2475=ORIENTED_EDGE('',*,*,#4158,.F.);
#2476=ORIENTED_EDGE('',*,*,#4157,.F.);
#2477=ORIENTED_EDGE('',*,*,#4173,.F.);
#2478=ORIENTED_EDGE('',*,*,#4174,.F.);
#2479=ORIENTED_EDGE('',*,*,#4175,.F.);
#2480=ORIENTED_EDGE('',*,*,#4159,.F.);
#2481=ORIENTED_EDGE('',*,*,#4172,.T.);
#2482=ORIENTED_EDGE('',*,*,#4160,.F.);
#2483=ORIENTED_EDGE('',*,*,#4175,.T.);
#2484=ORIENTED_EDGE('',*,*,#4176,.F.);
#2485=ORIENTED_EDGE('',*,*,#4177,.F.);
#2486=ORIENTED_EDGE('',*,*,#4161,.F.);
#2487=ORIENTED_EDGE('',*,*,#4177,.T.);
#2488=ORIENTED_EDGE('',*,*,#4178,.F.);
#2489=ORIENTED_EDGE('',*,*,#4179,.F.);
#2490=ORIENTED_EDGE('',*,*,#4162,.F.);
#2491=ORIENTED_EDGE('',*,*,#4179,.T.);
#2492=ORIENTED_EDGE('',*,*,#4180,.F.);
#2493=ORIENTED_EDGE('',*,*,#4181,.F.);
#2494=ORIENTED_EDGE('',*,*,#4163,.F.);
#2495=ORIENTED_EDGE('',*,*,#4181,.T.);
#2496=ORIENTED_EDGE('',*,*,#4182,.F.);
#2497=ORIENTED_EDGE('',*,*,#4183,.F.);
#2498=ORIENTED_EDGE('',*,*,#4164,.F.);
#2499=ORIENTED_EDGE('',*,*,#4183,.T.);
#2500=ORIENTED_EDGE('',*,*,#4184,.F.);
#2501=ORIENTED_EDGE('',*,*,#4185,.F.);
#2502=ORIENTED_EDGE('',*,*,#4165,.F.);
#2503=ORIENTED_EDGE('',*,*,#4185,.T.);
#2504=ORIENTED_EDGE('',*,*,#4186,.F.);
#2505=ORIENTED_EDGE('',*,*,#4187,.F.);
#2506=ORIENTED_EDGE('',*,*,#4166,.F.);
#2507=ORIENTED_EDGE('',*,*,#4187,.T.);
#2508=ORIENTED_EDGE('',*,*,#4188,.F.);
#2509=ORIENTED_EDGE('',*,*,#4189,.F.);
#2510=ORIENTED_EDGE('',*,*,#4167,.F.);
#2511=ORIENTED_EDGE('',*,*,#4189,.T.);
#2512=ORIENTED_EDGE('',*,*,#4190,.F.);
#2513=ORIENTED_EDGE('',*,*,#4191,.F.);
#2514=ORIENTED_EDGE('',*,*,#4168,.F.);
#2515=ORIENTED_EDGE('',*,*,#4191,.T.);
#2516=ORIENTED_EDGE('',*,*,#4192,.F.);
#2517=ORIENTED_EDGE('',*,*,#4193,.F.);
#2518=ORIENTED_EDGE('',*,*,#4169,.F.);
#2519=ORIENTED_EDGE('',*,*,#4193,.T.);
#2520=ORIENTED_EDGE('',*,*,#4194,.F.);
#2521=ORIENTED_EDGE('',*,*,#4195,.F.);
#2522=ORIENTED_EDGE('',*,*,#4195,.T.);
#2523=ORIENTED_EDGE('',*,*,#4196,.F.);
#2524=ORIENTED_EDGE('',*,*,#4197,.F.);
#2525=ORIENTED_EDGE('',*,*,#4144,.F.);
#2526=ORIENTED_EDGE('',*,*,#4145,.F.);
#2527=ORIENTED_EDGE('',*,*,#4197,.T.);
#2528=ORIENTED_EDGE('',*,*,#4198,.F.);
#2529=ORIENTED_EDGE('',*,*,#4199,.F.);
#2530=ORIENTED_EDGE('',*,*,#4200,.F.);
#2531=ORIENTED_EDGE('',*,*,#4201,.F.);
#2532=ORIENTED_EDGE('',*,*,#4146,.F.);
#2533=ORIENTED_EDGE('',*,*,#4199,.T.);
#2534=ORIENTED_EDGE('',*,*,#4202,.F.);
#2535=ORIENTED_EDGE('',*,*,#4203,.F.);
#2536=ORIENTED_EDGE('',*,*,#4147,.F.);
#2537=ORIENTED_EDGE('',*,*,#4201,.T.);
#2538=ORIENTED_EDGE('',*,*,#4204,.F.);
#2539=ORIENTED_EDGE('',*,*,#4205,.F.);
#2540=ORIENTED_EDGE('',*,*,#4148,.F.);
#2541=ORIENTED_EDGE('',*,*,#4203,.T.);
#2542=ORIENTED_EDGE('',*,*,#4206,.F.);
#2543=ORIENTED_EDGE('',*,*,#4207,.F.);
#2544=ORIENTED_EDGE('',*,*,#4149,.F.);
#2545=ORIENTED_EDGE('',*,*,#4205,.T.);
#2546=ORIENTED_EDGE('',*,*,#4208,.F.);
#2547=ORIENTED_EDGE('',*,*,#4209,.F.);
#2548=ORIENTED_EDGE('',*,*,#4150,.F.);
#2549=ORIENTED_EDGE('',*,*,#4207,.T.);
#2550=ORIENTED_EDGE('',*,*,#4210,.F.);
#2551=ORIENTED_EDGE('',*,*,#4211,.F.);
#2552=ORIENTED_EDGE('',*,*,#4151,.F.);
#2553=ORIENTED_EDGE('',*,*,#4209,.T.);
#2554=ORIENTED_EDGE('',*,*,#4212,.F.);
#2555=ORIENTED_EDGE('',*,*,#4213,.F.);
#2556=ORIENTED_EDGE('',*,*,#4152,.F.);
#2557=ORIENTED_EDGE('',*,*,#4211,.T.);
#2558=ORIENTED_EDGE('',*,*,#4214,.F.);
#2559=ORIENTED_EDGE('',*,*,#4215,.F.);
#2560=ORIENTED_EDGE('',*,*,#4153,.F.);
#2561=ORIENTED_EDGE('',*,*,#4213,.T.);
#2562=ORIENTED_EDGE('',*,*,#4216,.F.);
#2563=ORIENTED_EDGE('',*,*,#4217,.F.);
#2564=ORIENTED_EDGE('',*,*,#4154,.F.);
#2565=ORIENTED_EDGE('',*,*,#4215,.T.);
#2566=ORIENTED_EDGE('',*,*,#4218,.F.);
#2567=ORIENTED_EDGE('',*,*,#4219,.F.);
#2568=ORIENTED_EDGE('',*,*,#4155,.F.);
#2569=ORIENTED_EDGE('',*,*,#4217,.T.);
#2570=ORIENTED_EDGE('',*,*,#4220,.F.);
#2571=ORIENTED_EDGE('',*,*,#4173,.T.);
#2572=ORIENTED_EDGE('',*,*,#4156,.F.);
#2573=ORIENTED_EDGE('',*,*,#4219,.T.);
#2574=ORIENTED_EDGE('',*,*,#4221,.F.);
#2575=ORIENTED_EDGE('',*,*,#4170,.F.);
#2576=ORIENTED_EDGE('',*,*,#4222,.T.);
#2577=ORIENTED_EDGE('',*,*,#4171,.T.);
#2578=ORIENTED_EDGE('',*,*,#4223,.T.);
#2579=ORIENTED_EDGE('',*,*,#4224,.T.);
#2580=ORIENTED_EDGE('',*,*,#4225,.F.);
#2581=ORIENTED_EDGE('',*,*,#4226,.F.);
#2582=ORIENTED_EDGE('',*,*,#4227,.F.);
#2583=ORIENTED_EDGE('',*,*,#4174,.T.);
#2584=ORIENTED_EDGE('',*,*,#4222,.F.);
#2585=ORIENTED_EDGE('',*,*,#4228,.F.);
#2586=ORIENTED_EDGE('',*,*,#4229,.F.);
#2587=ORIENTED_EDGE('',*,*,#4230,.F.);
#2588=ORIENTED_EDGE('',*,*,#4192,.T.);
#2589=ORIENTED_EDGE('',*,*,#4231,.F.);
#2590=ORIENTED_EDGE('',*,*,#4232,.F.);
#2591=ORIENTED_EDGE('',*,*,#4233,.F.);
#2592=ORIENTED_EDGE('',*,*,#4234,.F.);
#2593=ORIENTED_EDGE('',*,*,#4235,.F.);
#2594=ORIENTED_EDGE('',*,*,#4236,.F.);
#2595=ORIENTED_EDGE('',*,*,#4237,.F.);
#2596=ORIENTED_EDGE('',*,*,#4184,.T.);
#2597=ORIENTED_EDGE('',*,*,#4238,.F.);
#2598=ORIENTED_EDGE('',*,*,#4239,.F.);
#2599=ORIENTED_EDGE('',*,*,#4240,.F.);
#2600=ORIENTED_EDGE('',*,*,#4241,.F.);
#2601=ORIENTED_EDGE('',*,*,#4242,.F.);
#2602=ORIENTED_EDGE('',*,*,#4243,.F.);
#2603=ORIENTED_EDGE('',*,*,#4244,.F.);
#2604=ORIENTED_EDGE('',*,*,#4176,.T.);
#2605=ORIENTED_EDGE('',*,*,#4227,.T.);
#2606=ORIENTED_EDGE('',*,*,#4245,.F.);
#2607=ORIENTED_EDGE('',*,*,#4246,.F.);
#2608=ORIENTED_EDGE('',*,*,#4247,.F.);
#2609=ORIENTED_EDGE('',*,*,#4248,.F.);
#2610=ORIENTED_EDGE('',*,*,#4249,.F.);
#2611=ORIENTED_EDGE('',*,*,#4250,.F.);
#2612=ORIENTED_EDGE('',*,*,#4218,.T.);
#2613=ORIENTED_EDGE('',*,*,#4251,.F.);
#2614=ORIENTED_EDGE('',*,*,#4252,.F.);
#2615=ORIENTED_EDGE('',*,*,#4253,.F.);
#2616=ORIENTED_EDGE('',*,*,#4254,.F.);
#2617=ORIENTED_EDGE('',*,*,#4255,.F.);
#2618=ORIENTED_EDGE('',*,*,#4256,.F.);
#2619=ORIENTED_EDGE('',*,*,#4257,.F.);
#2620=ORIENTED_EDGE('',*,*,#4210,.T.);
#2621=ORIENTED_EDGE('',*,*,#4258,.F.);
#2622=ORIENTED_EDGE('',*,*,#4259,.F.);
#2623=ORIENTED_EDGE('',*,*,#4260,.F.);
#2624=ORIENTED_EDGE('',*,*,#4261,.F.);
#2625=ORIENTED_EDGE('',*,*,#4262,.F.);
#2626=ORIENTED_EDGE('',*,*,#4263,.F.);
#2627=ORIENTED_EDGE('',*,*,#4264,.F.);
#2628=ORIENTED_EDGE('',*,*,#4202,.T.);
#2629=ORIENTED_EDGE('',*,*,#4265,.F.);
#2630=ORIENTED_EDGE('',*,*,#4266,.F.);
#2631=ORIENTED_EDGE('',*,*,#4267,.F.);
#2632=ORIENTED_EDGE('',*,*,#4268,.F.);
#2633=ORIENTED_EDGE('',*,*,#4269,.F.);
#2634=ORIENTED_EDGE('',*,*,#4270,.F.);
#2635=ORIENTED_EDGE('',*,*,#4271,.F.);
#2636=ORIENTED_EDGE('',*,*,#4272,.F.);
#2637=ORIENTED_EDGE('',*,*,#4273,.F.);
#2638=ORIENTED_EDGE('',*,*,#4274,.F.);
#2639=ORIENTED_EDGE('',*,*,#4275,.F.);
#2640=ORIENTED_EDGE('',*,*,#4276,.F.);
#2641=ORIENTED_EDGE('',*,*,#4277,.F.);
#2642=ORIENTED_EDGE('',*,*,#4278,.F.);
#2643=ORIENTED_EDGE('',*,*,#4279,.F.);
#2644=ORIENTED_EDGE('',*,*,#4280,.F.);
#2645=ORIENTED_EDGE('',*,*,#4281,.F.);
#2646=ORIENTED_EDGE('',*,*,#4282,.F.);
#2647=ORIENTED_EDGE('',*,*,#4283,.F.);
#2648=ORIENTED_EDGE('',*,*,#4284,.F.);
#2649=ORIENTED_EDGE('',*,*,#4285,.F.);
#2650=ORIENTED_EDGE('',*,*,#4286,.F.);
#2651=ORIENTED_EDGE('',*,*,#4287,.F.);
#2652=ORIENTED_EDGE('',*,*,#4244,.T.);
#2653=ORIENTED_EDGE('',*,*,#4288,.F.);
#2654=ORIENTED_EDGE('',*,*,#4289,.F.);
#2655=ORIENTED_EDGE('',*,*,#4290,.F.);
#2656=ORIENTED_EDGE('',*,*,#4178,.T.);
#2657=ORIENTED_EDGE('',*,*,#4291,.T.);
#2658=ORIENTED_EDGE('',*,*,#4180,.T.);
#2659=ORIENTED_EDGE('',*,*,#4290,.T.);
#2660=ORIENTED_EDGE('',*,*,#4292,.T.);
#2661=ORIENTED_EDGE('',*,*,#4182,.T.);
#2662=ORIENTED_EDGE('',*,*,#4291,.F.);
#2663=ORIENTED_EDGE('',*,*,#4293,.F.);
#2664=ORIENTED_EDGE('',*,*,#4294,.F.);
#2665=ORIENTED_EDGE('',*,*,#4238,.T.);
#2666=ORIENTED_EDGE('',*,*,#4237,.T.);
#2667=ORIENTED_EDGE('',*,*,#4295,.F.);
#2668=ORIENTED_EDGE('',*,*,#4296,.F.);
#2669=ORIENTED_EDGE('',*,*,#4297,.F.);
#2670=ORIENTED_EDGE('',*,*,#4186,.T.);
#2671=ORIENTED_EDGE('',*,*,#4297,.T.);
#2672=ORIENTED_EDGE('',*,*,#4298,.T.);
#2673=ORIENTED_EDGE('',*,*,#4299,.T.);
#2674=ORIENTED_EDGE('',*,*,#4188,.T.);
#2675=ORIENTED_EDGE('',*,*,#4190,.T.);
#2676=ORIENTED_EDGE('',*,*,#4299,.F.);
#2677=ORIENTED_EDGE('',*,*,#4300,.F.);
#2678=ORIENTED_EDGE('',*,*,#4301,.F.);
#2679=ORIENTED_EDGE('',*,*,#4231,.T.);
#2680=ORIENTED_EDGE('',*,*,#4230,.T.);
#2681=ORIENTED_EDGE('',*,*,#4302,.F.);
#2682=ORIENTED_EDGE('',*,*,#4303,.F.);
#2683=ORIENTED_EDGE('',*,*,#4304,.F.);
#2684=ORIENTED_EDGE('',*,*,#4194,.T.);
#2685=ORIENTED_EDGE('',*,*,#4305,.T.);
#2686=ORIENTED_EDGE('',*,*,#4306,.T.);
#2687=ORIENTED_EDGE('',*,*,#4198,.T.);
#2688=ORIENTED_EDGE('',*,*,#4196,.T.);
#2689=ORIENTED_EDGE('',*,*,#4304,.T.);
#2690=ORIENTED_EDGE('',*,*,#4200,.T.);
#2691=ORIENTED_EDGE('',*,*,#4306,.F.);
#2692=ORIENTED_EDGE('',*,*,#4307,.F.);
#2693=ORIENTED_EDGE('',*,*,#4308,.F.);
#2694=ORIENTED_EDGE('',*,*,#4265,.T.);
#2695=ORIENTED_EDGE('',*,*,#4264,.T.);
#2696=ORIENTED_EDGE('',*,*,#4309,.F.);
#2697=ORIENTED_EDGE('',*,*,#4310,.F.);
#2698=ORIENTED_EDGE('',*,*,#4311,.F.);
#2699=ORIENTED_EDGE('',*,*,#4204,.T.);
#2700=ORIENTED_EDGE('',*,*,#4311,.T.);
#2701=ORIENTED_EDGE('',*,*,#4312,.T.);
#2702=ORIENTED_EDGE('',*,*,#4313,.T.);
#2703=ORIENTED_EDGE('',*,*,#4206,.T.);
#2704=ORIENTED_EDGE('',*,*,#4208,.T.);
#2705=ORIENTED_EDGE('',*,*,#4313,.F.);
#2706=ORIENTED_EDGE('',*,*,#4314,.F.);
#2707=ORIENTED_EDGE('',*,*,#4315,.F.);
#2708=ORIENTED_EDGE('',*,*,#4258,.T.);
#2709=ORIENTED_EDGE('',*,*,#4257,.T.);
#2710=ORIENTED_EDGE('',*,*,#4316,.F.);
#2711=ORIENTED_EDGE('',*,*,#4317,.F.);
#2712=ORIENTED_EDGE('',*,*,#4318,.F.);
#2713=ORIENTED_EDGE('',*,*,#4212,.T.);
#2714=ORIENTED_EDGE('',*,*,#4319,.T.);
#2715=ORIENTED_EDGE('',*,*,#4214,.T.);
#2716=ORIENTED_EDGE('',*,*,#4318,.T.);
#2717=ORIENTED_EDGE('',*,*,#4320,.T.);
#2718=ORIENTED_EDGE('',*,*,#4216,.T.);
#2719=ORIENTED_EDGE('',*,*,#4319,.F.);
#2720=ORIENTED_EDGE('',*,*,#4321,.F.);
#2721=ORIENTED_EDGE('',*,*,#4322,.F.);
#2722=ORIENTED_EDGE('',*,*,#4251,.T.);
#2723=ORIENTED_EDGE('',*,*,#4323,.F.);
#2724=ORIENTED_EDGE('',*,*,#4223,.F.);
#2725=ORIENTED_EDGE('',*,*,#4220,.T.);
#2726=ORIENTED_EDGE('',*,*,#4250,.T.);
#2727=ORIENTED_EDGE('',*,*,#4324,.F.);
#2728=ORIENTED_EDGE('',*,*,#4325,.T.);
#2729=ORIENTED_EDGE('',*,*,#4326,.T.);
#2730=ORIENTED_EDGE('',*,*,#4221,.T.);
#2731=ORIENTED_EDGE('',*,*,#4327,.F.);
#2732=ORIENTED_EDGE('',*,*,#4328,.F.);
#2733=ORIENTED_EDGE('',*,*,#4329,.F.);
#2734=ORIENTED_EDGE('',*,*,#4330,.F.);
#2735=ORIENTED_EDGE('',*,*,#4293,.T.);
#2736=ORIENTED_EDGE('',*,*,#4292,.F.);
#2737=ORIENTED_EDGE('',*,*,#4289,.T.);
#2738=ORIENTED_EDGE('',*,*,#4331,.F.);
#2739=ORIENTED_EDGE('',*,*,#4332,.F.);
#2740=ORIENTED_EDGE('',*,*,#4333,.F.);
#2741=ORIENTED_EDGE('',*,*,#4296,.T.);
#2742=ORIENTED_EDGE('',*,*,#4334,.F.);
#2743=ORIENTED_EDGE('',*,*,#4335,.F.);
#2744=ORIENTED_EDGE('',*,*,#4336,.F.);
#2745=ORIENTED_EDGE('',*,*,#4337,.F.);
#2746=ORIENTED_EDGE('',*,*,#4338,.F.);
#2747=ORIENTED_EDGE('',*,*,#4300,.T.);
#2748=ORIENTED_EDGE('',*,*,#4298,.F.);
#2749=ORIENTED_EDGE('',*,*,#4303,.T.);
#2750=ORIENTED_EDGE('',*,*,#4339,.F.);
#2751=ORIENTED_EDGE('',*,*,#4340,.F.);
#2752=ORIENTED_EDGE('',*,*,#4341,.F.);
#2753=ORIENTED_EDGE('',*,*,#4342,.F.);
#2754=ORIENTED_EDGE('',*,*,#4343,.F.);
#2755=ORIENTED_EDGE('',*,*,#4307,.T.);
#2756=ORIENTED_EDGE('',*,*,#4305,.F.);
#2757=ORIENTED_EDGE('',*,*,#4310,.T.);
#2758=ORIENTED_EDGE('',*,*,#4344,.F.);
#2759=ORIENTED_EDGE('',*,*,#4345,.F.);
#2760=ORIENTED_EDGE('',*,*,#4346,.F.);
#2761=ORIENTED_EDGE('',*,*,#4347,.F.);
#2762=ORIENTED_EDGE('',*,*,#4348,.F.);
#2763=ORIENTED_EDGE('',*,*,#4314,.T.);
#2764=ORIENTED_EDGE('',*,*,#4312,.F.);
#2765=ORIENTED_EDGE('',*,*,#4317,.T.);
#2766=ORIENTED_EDGE('',*,*,#4349,.F.);
#2767=ORIENTED_EDGE('',*,*,#4350,.F.);
#2768=ORIENTED_EDGE('',*,*,#4351,.F.);
#2769=ORIENTED_EDGE('',*,*,#4352,.F.);
#2770=ORIENTED_EDGE('',*,*,#4353,.F.);
#2771=ORIENTED_EDGE('',*,*,#4321,.T.);
#2772=ORIENTED_EDGE('',*,*,#4320,.F.);
#2773=ORIENTED_EDGE('',*,*,#4354,.F.);
#2774=ORIENTED_EDGE('',*,*,#4355,.F.);
#2775=ORIENTED_EDGE('',*,*,#4225,.T.);
#2776=ORIENTED_EDGE('',*,*,#4224,.F.);
#2777=ORIENTED_EDGE('',*,*,#4323,.T.);
#2778=ORIENTED_EDGE('',*,*,#4356,.F.);
#2779=ORIENTED_EDGE('',*,*,#4357,.F.);
#2780=ORIENTED_EDGE('',*,*,#4358,.F.);
#2781=ORIENTED_EDGE('',*,*,#4359,.F.);
#2782=ORIENTED_EDGE('',*,*,#4360,.F.);
#2783=ORIENTED_EDGE('',*,*,#4361,.F.);
#2784=ORIENTED_EDGE('',*,*,#4362,.F.);
#2785=ORIENTED_EDGE('',*,*,#4363,.F.);
#2786=ORIENTED_EDGE('',*,*,#4364,.F.);
#2787=ORIENTED_EDGE('',*,*,#4365,.F.);
#2788=ORIENTED_EDGE('',*,*,#4366,.F.);
#2789=ORIENTED_EDGE('',*,*,#4367,.F.);
#2790=ORIENTED_EDGE('',*,*,#4368,.F.);
#2791=ORIENTED_EDGE('',*,*,#4369,.F.);
#2792=ORIENTED_EDGE('',*,*,#4370,.F.);
#2793=ORIENTED_EDGE('',*,*,#4371,.F.);
#2794=ORIENTED_EDGE('',*,*,#4372,.F.);
#2795=ORIENTED_EDGE('',*,*,#4373,.F.);
#2796=ORIENTED_EDGE('',*,*,#4374,.F.);
#2797=ORIENTED_EDGE('',*,*,#4375,.F.);
#2798=ORIENTED_EDGE('',*,*,#4376,.F.);
#2799=ORIENTED_EDGE('',*,*,#4377,.F.);
#2800=ORIENTED_EDGE('',*,*,#4245,.T.);
#2801=ORIENTED_EDGE('',*,*,#4226,.T.);
#2802=ORIENTED_EDGE('',*,*,#4355,.T.);
#2803=ORIENTED_EDGE('',*,*,#4287,.T.);
#2804=ORIENTED_EDGE('',*,*,#4376,.T.);
#2805=ORIENTED_EDGE('',*,*,#4375,.T.);
#2806=ORIENTED_EDGE('',*,*,#4286,.T.);
#2807=ORIENTED_EDGE('',*,*,#4285,.T.);
#2808=ORIENTED_EDGE('',*,*,#4374,.T.);
#2809=ORIENTED_EDGE('',*,*,#4284,.T.);
#2810=ORIENTED_EDGE('',*,*,#4373,.T.);
#2811=ORIENTED_EDGE('',*,*,#4283,.T.);
#2812=ORIENTED_EDGE('',*,*,#4372,.T.);
#2813=ORIENTED_EDGE('',*,*,#4282,.T.);
#2814=ORIENTED_EDGE('',*,*,#4371,.T.);
#2815=ORIENTED_EDGE('',*,*,#4281,.T.);
#2816=ORIENTED_EDGE('',*,*,#4370,.T.);
#2817=ORIENTED_EDGE('',*,*,#4280,.T.);
#2818=ORIENTED_EDGE('',*,*,#4369,.T.);
#2819=ORIENTED_EDGE('',*,*,#4279,.T.);
#2820=ORIENTED_EDGE('',*,*,#4368,.T.);
#2821=ORIENTED_EDGE('',*,*,#4278,.T.);
#2822=ORIENTED_EDGE('',*,*,#4367,.T.);
#2823=ORIENTED_EDGE('',*,*,#4277,.T.);
#2824=ORIENTED_EDGE('',*,*,#4366,.T.);
#2825=ORIENTED_EDGE('',*,*,#4276,.T.);
#2826=ORIENTED_EDGE('',*,*,#4365,.T.);
#2827=ORIENTED_EDGE('',*,*,#4275,.T.);
#2828=ORIENTED_EDGE('',*,*,#4364,.T.);
#2829=ORIENTED_EDGE('',*,*,#4274,.T.);
#2830=ORIENTED_EDGE('',*,*,#4363,.T.);
#2831=ORIENTED_EDGE('',*,*,#4273,.T.);
#2832=ORIENTED_EDGE('',*,*,#4362,.T.);
#2833=ORIENTED_EDGE('',*,*,#4272,.T.);
#2834=ORIENTED_EDGE('',*,*,#4361,.T.);
#2835=ORIENTED_EDGE('',*,*,#4271,.T.);
#2836=ORIENTED_EDGE('',*,*,#4360,.T.);
#2837=ORIENTED_EDGE('',*,*,#4270,.T.);
#2838=ORIENTED_EDGE('',*,*,#4359,.T.);
#2839=ORIENTED_EDGE('',*,*,#4378,.F.);
#2840=ORIENTED_EDGE('',*,*,#4232,.T.);
#2841=ORIENTED_EDGE('',*,*,#4301,.T.);
#2842=ORIENTED_EDGE('',*,*,#4338,.T.);
#2843=ORIENTED_EDGE('',*,*,#4378,.T.);
#2844=ORIENTED_EDGE('',*,*,#4337,.T.);
#2845=ORIENTED_EDGE('',*,*,#4379,.F.);
#2846=ORIENTED_EDGE('',*,*,#4233,.T.);
#2847=ORIENTED_EDGE('',*,*,#4234,.T.);
#2848=ORIENTED_EDGE('',*,*,#4379,.T.);
#2849=ORIENTED_EDGE('',*,*,#4336,.T.);
#2850=ORIENTED_EDGE('',*,*,#4380,.F.);
#2851=ORIENTED_EDGE('',*,*,#4235,.T.);
#2852=ORIENTED_EDGE('',*,*,#4380,.T.);
#2853=ORIENTED_EDGE('',*,*,#4335,.T.);
#2854=ORIENTED_EDGE('',*,*,#4381,.F.);
#2855=ORIENTED_EDGE('',*,*,#4381,.T.);
#2856=ORIENTED_EDGE('',*,*,#4334,.T.);
#2857=ORIENTED_EDGE('',*,*,#4295,.T.);
#2858=ORIENTED_EDGE('',*,*,#4236,.T.);
#2859=ORIENTED_EDGE('',*,*,#4382,.F.);
#2860=ORIENTED_EDGE('',*,*,#4239,.T.);
#2861=ORIENTED_EDGE('',*,*,#4294,.T.);
#2862=ORIENTED_EDGE('',*,*,#4330,.T.);
#2863=ORIENTED_EDGE('',*,*,#4382,.T.);
#2864=ORIENTED_EDGE('',*,*,#4329,.T.);
#2865=ORIENTED_EDGE('',*,*,#4383,.F.);
#2866=ORIENTED_EDGE('',*,*,#4240,.T.);
#2867=ORIENTED_EDGE('',*,*,#4241,.T.);
#2868=ORIENTED_EDGE('',*,*,#4383,.T.);
#2869=ORIENTED_EDGE('',*,*,#4333,.T.);
#2870=ORIENTED_EDGE('',*,*,#4384,.F.);
#2871=ORIENTED_EDGE('',*,*,#4242,.T.);
#2872=ORIENTED_EDGE('',*,*,#4384,.T.);
#2873=ORIENTED_EDGE('',*,*,#4332,.T.);
#2874=ORIENTED_EDGE('',*,*,#4385,.F.);
#2875=ORIENTED_EDGE('',*,*,#4385,.T.);
#2876=ORIENTED_EDGE('',*,*,#4331,.T.);
#2877=ORIENTED_EDGE('',*,*,#4288,.T.);
#2878=ORIENTED_EDGE('',*,*,#4243,.T.);
#2879=ORIENTED_EDGE('',*,*,#4246,.T.);
#2880=ORIENTED_EDGE('',*,*,#4377,.T.);
#2881=ORIENTED_EDGE('',*,*,#4354,.T.);
#2882=ORIENTED_EDGE('',*,*,#4386,.F.);
#2883=ORIENTED_EDGE('',*,*,#4247,.T.);
#2884=ORIENTED_EDGE('',*,*,#4386,.T.);
#2885=ORIENTED_EDGE('',*,*,#4358,.T.);
#2886=ORIENTED_EDGE('',*,*,#4387,.F.);
#2887=ORIENTED_EDGE('',*,*,#4248,.T.);
#2888=ORIENTED_EDGE('',*,*,#4387,.T.);
#2889=ORIENTED_EDGE('',*,*,#4357,.T.);
#2890=ORIENTED_EDGE('',*,*,#4388,.F.);
#2891=ORIENTED_EDGE('',*,*,#4388,.T.);
#2892=ORIENTED_EDGE('',*,*,#4356,.T.);
#2893=ORIENTED_EDGE('',*,*,#4324,.T.);
#2894=ORIENTED_EDGE('',*,*,#4249,.T.);
#2895=ORIENTED_EDGE('',*,*,#4389,.F.);
#2896=ORIENTED_EDGE('',*,*,#4252,.T.);
#2897=ORIENTED_EDGE('',*,*,#4322,.T.);
#2898=ORIENTED_EDGE('',*,*,#4353,.T.);
#2899=ORIENTED_EDGE('',*,*,#4253,.T.);
#2900=ORIENTED_EDGE('',*,*,#4389,.T.);
#2901=ORIENTED_EDGE('',*,*,#4352,.T.);
#2902=ORIENTED_EDGE('',*,*,#4390,.F.);
#2903=ORIENTED_EDGE('',*,*,#4351,.T.);
#2904=ORIENTED_EDGE('',*,*,#4391,.F.);
#2905=ORIENTED_EDGE('',*,*,#4254,.T.);
#2906=ORIENTED_EDGE('',*,*,#4390,.T.);
#2907=ORIENTED_EDGE('',*,*,#4391,.T.);
#2908=ORIENTED_EDGE('',*,*,#4350,.T.);
#2909=ORIENTED_EDGE('',*,*,#4392,.F.);
#2910=ORIENTED_EDGE('',*,*,#4255,.T.);
#2911=ORIENTED_EDGE('',*,*,#4392,.T.);
#2912=ORIENTED_EDGE('',*,*,#4349,.T.);
#2913=ORIENTED_EDGE('',*,*,#4316,.T.);
#2914=ORIENTED_EDGE('',*,*,#4256,.T.);
#2915=ORIENTED_EDGE('',*,*,#4393,.F.);
#2916=ORIENTED_EDGE('',*,*,#4259,.T.);
#2917=ORIENTED_EDGE('',*,*,#4315,.T.);
#2918=ORIENTED_EDGE('',*,*,#4348,.T.);
#2919=ORIENTED_EDGE('',*,*,#4260,.T.);
#2920=ORIENTED_EDGE('',*,*,#4393,.T.);
#2921=ORIENTED_EDGE('',*,*,#4347,.T.);
#2922=ORIENTED_EDGE('',*,*,#4394,.F.);
#2923=ORIENTED_EDGE('',*,*,#4346,.T.);
#2924=ORIENTED_EDGE('',*,*,#4395,.F.);
#2925=ORIENTED_EDGE('',*,*,#4261,.T.);
#2926=ORIENTED_EDGE('',*,*,#4394,.T.);
#2927=ORIENTED_EDGE('',*,*,#4395,.T.);
#2928=ORIENTED_EDGE('',*,*,#4345,.T.);
#2929=ORIENTED_EDGE('',*,*,#4396,.F.);
#2930=ORIENTED_EDGE('',*,*,#4262,.T.);
#2931=ORIENTED_EDGE('',*,*,#4396,.T.);
#2932=ORIENTED_EDGE('',*,*,#4344,.T.);
#2933=ORIENTED_EDGE('',*,*,#4309,.T.);
#2934=ORIENTED_EDGE('',*,*,#4263,.T.);
#2935=ORIENTED_EDGE('',*,*,#4397,.F.);
#2936=ORIENTED_EDGE('',*,*,#4266,.T.);
#2937=ORIENTED_EDGE('',*,*,#4308,.T.);
#2938=ORIENTED_EDGE('',*,*,#4343,.T.);
#2939=ORIENTED_EDGE('',*,*,#4267,.T.);
#2940=ORIENTED_EDGE('',*,*,#4397,.T.);
#2941=ORIENTED_EDGE('',*,*,#4342,.T.);
#2942=ORIENTED_EDGE('',*,*,#4398,.F.);
#2943=ORIENTED_EDGE('',*,*,#4398,.T.);
#2944=ORIENTED_EDGE('',*,*,#4341,.T.);
#2945=ORIENTED_EDGE('',*,*,#4399,.F.);
#2946=ORIENTED_EDGE('',*,*,#4268,.T.);
#2947=ORIENTED_EDGE('',*,*,#4269,.T.);
#2948=ORIENTED_EDGE('',*,*,#4399,.T.);
#2949=ORIENTED_EDGE('',*,*,#4340,.T.);
#2950=ORIENTED_EDGE('',*,*,#4400,.F.);
#2951=ORIENTED_EDGE('',*,*,#4400,.T.);
#2952=ORIENTED_EDGE('',*,*,#4339,.T.);
#2953=ORIENTED_EDGE('',*,*,#4302,.T.);
#2954=ORIENTED_EDGE('',*,*,#4229,.T.);
#2955=ORIENTED_EDGE('',*,*,#4401,.T.);
#2956=ORIENTED_EDGE('',*,*,#4402,.T.);
#2957=ORIENTED_EDGE('',*,*,#4228,.T.);
#2958=ORIENTED_EDGE('',*,*,#4403,.T.);
#2959=ORIENTED_EDGE('',*,*,#4404,.T.);
#2960=ORIENTED_EDGE('',*,*,#4326,.F.);
#2961=ORIENTED_EDGE('',*,*,#4325,.F.);
#2962=ORIENTED_EDGE('',*,*,#4405,.F.);
#2963=ORIENTED_EDGE('',*,*,#4406,.F.);
#2964=ORIENTED_EDGE('',*,*,#4328,.T.);
#2965=ORIENTED_EDGE('',*,*,#4407,.T.);
#2966=ORIENTED_EDGE('',*,*,#4408,.T.);
#2967=ORIENTED_EDGE('',*,*,#4327,.T.);
#2968=ORIENTED_EDGE('',*,*,#4401,.F.);
#2969=ORIENTED_EDGE('',*,*,#4402,.F.);
#2970=ORIENTED_EDGE('',*,*,#4408,.F.);
#2971=ORIENTED_EDGE('',*,*,#4407,.F.);
#2972=ORIENTED_EDGE('',*,*,#4409,.F.);
#2973=ORIENTED_EDGE('',*,*,#4404,.F.);
#2974=ORIENTED_EDGE('',*,*,#4403,.F.);
#2975=ORIENTED_EDGE('',*,*,#4406,.T.);
#2976=ORIENTED_EDGE('',*,*,#4405,.T.);
#2977=ORIENTED_EDGE('',*,*,#4410,.T.);
#2978=ORIENTED_EDGE('',*,*,#4411,.T.);
#2979=ORIENTED_EDGE('',*,*,#4412,.F.);
#2980=ORIENTED_EDGE('',*,*,#4413,.F.);
#2981=ORIENTED_EDGE('',*,*,#4414,.F.);
#2982=ORIENTED_EDGE('',*,*,#4415,.F.);
#2983=ORIENTED_EDGE('',*,*,#4416,.F.);
#2984=ORIENTED_EDGE('',*,*,#4417,.F.);
#2985=ORIENTED_EDGE('',*,*,#4418,.F.);
#2986=ORIENTED_EDGE('',*,*,#4419,.F.);
#2987=ORIENTED_EDGE('',*,*,#4420,.F.);
#2988=ORIENTED_EDGE('',*,*,#4421,.F.);
#2989=ORIENTED_EDGE('',*,*,#4422,.F.);
#2990=ORIENTED_EDGE('',*,*,#4423,.F.);
#2991=ORIENTED_EDGE('',*,*,#4424,.F.);
#2992=ORIENTED_EDGE('',*,*,#4425,.F.);
#2993=ORIENTED_EDGE('',*,*,#4426,.F.);
#2994=ORIENTED_EDGE('',*,*,#4427,.F.);
#2995=ORIENTED_EDGE('',*,*,#4428,.F.);
#2996=ORIENTED_EDGE('',*,*,#4429,.F.);
#2997=ORIENTED_EDGE('',*,*,#4430,.F.);
#2998=ORIENTED_EDGE('',*,*,#4431,.F.);
#2999=ORIENTED_EDGE('',*,*,#4432,.F.);
#3000=ORIENTED_EDGE('',*,*,#4433,.F.);
#3001=ORIENTED_EDGE('',*,*,#4434,.F.);
#3002=ORIENTED_EDGE('',*,*,#4435,.F.);
#3003=ORIENTED_EDGE('',*,*,#4436,.F.);
#3004=ORIENTED_EDGE('',*,*,#4437,.F.);
#3005=ORIENTED_EDGE('',*,*,#4438,.F.);
#3006=ORIENTED_EDGE('',*,*,#4439,.F.);
#3007=ORIENTED_EDGE('',*,*,#4440,.F.);
#3008=ORIENTED_EDGE('',*,*,#4441,.F.);
#3009=ORIENTED_EDGE('',*,*,#4442,.F.);
#3010=ORIENTED_EDGE('',*,*,#4443,.F.);
#3011=ORIENTED_EDGE('',*,*,#4409,.T.);
#3012=ORIENTED_EDGE('',*,*,#4410,.F.);
#3013=ORIENTED_EDGE('',*,*,#4444,.F.);
#3014=ORIENTED_EDGE('',*,*,#4445,.F.);
#3015=ORIENTED_EDGE('',*,*,#4446,.F.);
#3016=ORIENTED_EDGE('',*,*,#4447,.F.);
#3017=ORIENTED_EDGE('',*,*,#4448,.F.);
#3018=ORIENTED_EDGE('',*,*,#4449,.F.);
#3019=ORIENTED_EDGE('',*,*,#4450,.F.);
#3020=ORIENTED_EDGE('',*,*,#4451,.F.);
#3021=ORIENTED_EDGE('',*,*,#4452,.F.);
#3022=ORIENTED_EDGE('',*,*,#4453,.F.);
#3023=ORIENTED_EDGE('',*,*,#4454,.F.);
#3024=ORIENTED_EDGE('',*,*,#4455,.F.);
#3025=ORIENTED_EDGE('',*,*,#4456,.F.);
#3026=ORIENTED_EDGE('',*,*,#4457,.F.);
#3027=ORIENTED_EDGE('',*,*,#4458,.F.);
#3028=ORIENTED_EDGE('',*,*,#4459,.F.);
#3029=ORIENTED_EDGE('',*,*,#4460,.F.);
#3030=ORIENTED_EDGE('',*,*,#4444,.T.);
#3031=ORIENTED_EDGE('',*,*,#4411,.F.);
#3032=ORIENTED_EDGE('',*,*,#4458,.T.);
#3033=ORIENTED_EDGE('',*,*,#4461,.F.);
#3034=ORIENTED_EDGE('',*,*,#4462,.F.);
#3035=ORIENTED_EDGE('',*,*,#4463,.F.);
#3036=ORIENTED_EDGE('',*,*,#4464,.F.);
#3037=ORIENTED_EDGE('',*,*,#4465,.F.);
#3038=ORIENTED_EDGE('',*,*,#4466,.F.);
#3039=ORIENTED_EDGE('',*,*,#4467,.F.);
#3040=ORIENTED_EDGE('',*,*,#4468,.F.);
#3041=ORIENTED_EDGE('',*,*,#4469,.F.);
#3042=ORIENTED_EDGE('',*,*,#4470,.F.);
#3043=ORIENTED_EDGE('',*,*,#4471,.F.);
#3044=ORIENTED_EDGE('',*,*,#4443,.T.);
#3045=ORIENTED_EDGE('',*,*,#4472,.T.);
#3046=ORIENTED_EDGE('',*,*,#4473,.T.);
#3047=ORIENTED_EDGE('',*,*,#4474,.T.);
#3048=ORIENTED_EDGE('',*,*,#4475,.T.);
#3049=ORIENTED_EDGE('',*,*,#4442,.T.);
#3050=ORIENTED_EDGE('',*,*,#4476,.T.);
#3051=ORIENTED_EDGE('',*,*,#4475,.F.);
#3052=ORIENTED_EDGE('',*,*,#4477,.T.);
#3053=ORIENTED_EDGE('',*,*,#4476,.F.);
#3054=ORIENTED_EDGE('',*,*,#4441,.T.);
#3055=ORIENTED_EDGE('',*,*,#4478,.T.);
#3056=ORIENTED_EDGE('',*,*,#4479,.T.);
#3057=ORIENTED_EDGE('',*,*,#4480,.T.);
#3058=ORIENTED_EDGE('',*,*,#4440,.T.);
#3059=ORIENTED_EDGE('',*,*,#4481,.T.);
#3060=ORIENTED_EDGE('',*,*,#4482,.T.);
#3061=ORIENTED_EDGE('',*,*,#4483,.T.);
#3062=ORIENTED_EDGE('',*,*,#4439,.T.);
#3063=ORIENTED_EDGE('',*,*,#4484,.T.);
#3064=ORIENTED_EDGE('',*,*,#4485,.T.);
#3065=ORIENTED_EDGE('',*,*,#4438,.T.);
#3066=ORIENTED_EDGE('',*,*,#4486,.T.);
#3067=ORIENTED_EDGE('',*,*,#4485,.F.);
#3068=ORIENTED_EDGE('',*,*,#4487,.T.);
#3069=ORIENTED_EDGE('',*,*,#4486,.F.);
#3070=ORIENTED_EDGE('',*,*,#4437,.T.);
#3071=ORIENTED_EDGE('',*,*,#4488,.T.);
#3072=ORIENTED_EDGE('',*,*,#4489,.T.);
#3073=ORIENTED_EDGE('',*,*,#4436,.T.);
#3074=ORIENTED_EDGE('',*,*,#4464,.T.);
#3075=ORIENTED_EDGE('',*,*,#4490,.F.);
#3076=ORIENTED_EDGE('',*,*,#4491,.F.);
#3077=ORIENTED_EDGE('',*,*,#4492,.F.);
#3078=ORIENTED_EDGE('',*,*,#4413,.T.);
#3079=ORIENTED_EDGE('',*,*,#4493,.F.);
#3080=ORIENTED_EDGE('',*,*,#4494,.T.);
#3081=ORIENTED_EDGE('',*,*,#4495,.T.);
#3082=ORIENTED_EDGE('',*,*,#4496,.T.);
#3083=ORIENTED_EDGE('',*,*,#4497,.T.);
#3084=ORIENTED_EDGE('',*,*,#4414,.T.);
#3085=ORIENTED_EDGE('',*,*,#4492,.T.);
#3086=ORIENTED_EDGE('',*,*,#4415,.T.);
#3087=ORIENTED_EDGE('',*,*,#4497,.F.);
#3088=ORIENTED_EDGE('',*,*,#4498,.F.);
#3089=ORIENTED_EDGE('',*,*,#4499,.F.);
#3090=ORIENTED_EDGE('',*,*,#4462,.T.);
#3091=ORIENTED_EDGE('',*,*,#4500,.F.);
#3092=ORIENTED_EDGE('',*,*,#4500,.T.);
#3093=ORIENTED_EDGE('',*,*,#4461,.T.);
#3094=ORIENTED_EDGE('',*,*,#4457,.T.);
#3095=ORIENTED_EDGE('',*,*,#4501,.T.);
#3096=ORIENTED_EDGE('',*,*,#4416,.T.);
#3097=ORIENTED_EDGE('',*,*,#4456,.T.);
#3098=ORIENTED_EDGE('',*,*,#4502,.F.);
#3099=ORIENTED_EDGE('',*,*,#4503,.F.);
#3100=ORIENTED_EDGE('',*,*,#4504,.F.);
#3101=ORIENTED_EDGE('',*,*,#4417,.T.);
#3102=ORIENTED_EDGE('',*,*,#4501,.F.);
#3103=ORIENTED_EDGE('',*,*,#4505,.T.);
#3104=ORIENTED_EDGE('',*,*,#4506,.T.);
#3105=ORIENTED_EDGE('',*,*,#4507,.T.);
#3106=ORIENTED_EDGE('',*,*,#4508,.T.);
#3107=ORIENTED_EDGE('',*,*,#4418,.T.);
#3108=ORIENTED_EDGE('',*,*,#4504,.T.);
#3109=ORIENTED_EDGE('',*,*,#4419,.T.);
#3110=ORIENTED_EDGE('',*,*,#4508,.F.);
#3111=ORIENTED_EDGE('',*,*,#4509,.F.);
#3112=ORIENTED_EDGE('',*,*,#4510,.F.);
#3113=ORIENTED_EDGE('',*,*,#4454,.T.);
#3114=ORIENTED_EDGE('',*,*,#4511,.F.);
#3115=ORIENTED_EDGE('',*,*,#4453,.T.);
#3116=ORIENTED_EDGE('',*,*,#4512,.T.);
#3117=ORIENTED_EDGE('',*,*,#4513,.T.);
#3118=ORIENTED_EDGE('',*,*,#4420,.T.);
#3119=ORIENTED_EDGE('',*,*,#4511,.T.);
#3120=ORIENTED_EDGE('',*,*,#4421,.T.);
#3121=ORIENTED_EDGE('',*,*,#4513,.F.);
#3122=ORIENTED_EDGE('',*,*,#4514,.T.);
#3123=ORIENTED_EDGE('',*,*,#4515,.T.);
#3124=ORIENTED_EDGE('',*,*,#4516,.T.);
#3125=ORIENTED_EDGE('',*,*,#4517,.T.);
#3126=ORIENTED_EDGE('',*,*,#4518,.T.);
#3127=ORIENTED_EDGE('',*,*,#4519,.T.);
#3128=ORIENTED_EDGE('',*,*,#4422,.T.);
#3129=ORIENTED_EDGE('',*,*,#4520,.F.);
#3130=ORIENTED_EDGE('',*,*,#4423,.T.);
#3131=ORIENTED_EDGE('',*,*,#4519,.F.);
#3132=ORIENTED_EDGE('',*,*,#4521,.F.);
#3133=ORIENTED_EDGE('',*,*,#4522,.F.);
#3134=ORIENTED_EDGE('',*,*,#4450,.T.);
#3135=ORIENTED_EDGE('',*,*,#4449,.T.);
#3136=ORIENTED_EDGE('',*,*,#4523,.T.);
#3137=ORIENTED_EDGE('',*,*,#4424,.T.);
#3138=ORIENTED_EDGE('',*,*,#4520,.T.);
#3139=ORIENTED_EDGE('',*,*,#4448,.T.);
#3140=ORIENTED_EDGE('',*,*,#4524,.F.);
#3141=ORIENTED_EDGE('',*,*,#4525,.F.);
#3142=ORIENTED_EDGE('',*,*,#4526,.F.);
#3143=ORIENTED_EDGE('',*,*,#4425,.T.);
#3144=ORIENTED_EDGE('',*,*,#4523,.F.);
#3145=ORIENTED_EDGE('',*,*,#4527,.T.);
#3146=ORIENTED_EDGE('',*,*,#4528,.T.);
#3147=ORIENTED_EDGE('',*,*,#4529,.T.);
#3148=ORIENTED_EDGE('',*,*,#4530,.T.);
#3149=ORIENTED_EDGE('',*,*,#4426,.T.);
#3150=ORIENTED_EDGE('',*,*,#4526,.T.);
#3151=ORIENTED_EDGE('',*,*,#4427,.T.);
#3152=ORIENTED_EDGE('',*,*,#4530,.F.);
#3153=ORIENTED_EDGE('',*,*,#4531,.F.);
#3154=ORIENTED_EDGE('',*,*,#4532,.F.);
#3155=ORIENTED_EDGE('',*,*,#4446,.T.);
#3156=ORIENTED_EDGE('',*,*,#4533,.F.);
#3157=ORIENTED_EDGE('',*,*,#4460,.T.);
#3158=ORIENTED_EDGE('',*,*,#4534,.T.);
#3159=ORIENTED_EDGE('',*,*,#4428,.T.);
#3160=ORIENTED_EDGE('',*,*,#4533,.T.);
#3161=ORIENTED_EDGE('',*,*,#4445,.T.);
#3162=ORIENTED_EDGE('',*,*,#4459,.T.);
#3163=ORIENTED_EDGE('',*,*,#4535,.F.);
#3164=ORIENTED_EDGE('',*,*,#4536,.F.);
#3165=ORIENTED_EDGE('',*,*,#4537,.F.);
#3166=ORIENTED_EDGE('',*,*,#4429,.T.);
#3167=ORIENTED_EDGE('',*,*,#4534,.F.);
#3168=ORIENTED_EDGE('',*,*,#4538,.T.);
#3169=ORIENTED_EDGE('',*,*,#4539,.T.);
#3170=ORIENTED_EDGE('',*,*,#4540,.T.);
#3171=ORIENTED_EDGE('',*,*,#4541,.T.);
#3172=ORIENTED_EDGE('',*,*,#4430,.T.);
#3173=ORIENTED_EDGE('',*,*,#4537,.T.);
#3174=ORIENTED_EDGE('',*,*,#4431,.T.);
#3175=ORIENTED_EDGE('',*,*,#4541,.F.);
#3176=ORIENTED_EDGE('',*,*,#4542,.F.);
#3177=ORIENTED_EDGE('',*,*,#4543,.F.);
#3178=ORIENTED_EDGE('',*,*,#4470,.T.);
#3179=ORIENTED_EDGE('',*,*,#4544,.F.);
#3180=ORIENTED_EDGE('',*,*,#4469,.T.);
#3181=ORIENTED_EDGE('',*,*,#4545,.T.);
#3182=ORIENTED_EDGE('',*,*,#4432,.T.);
#3183=ORIENTED_EDGE('',*,*,#4544,.T.);
#3184=ORIENTED_EDGE('',*,*,#4468,.T.);
#3185=ORIENTED_EDGE('',*,*,#4546,.F.);
#3186=ORIENTED_EDGE('',*,*,#4547,.F.);
#3187=ORIENTED_EDGE('',*,*,#4548,.F.);
#3188=ORIENTED_EDGE('',*,*,#4433,.T.);
#3189=ORIENTED_EDGE('',*,*,#4545,.F.);
#3190=ORIENTED_EDGE('',*,*,#4549,.T.);
#3191=ORIENTED_EDGE('',*,*,#4550,.T.);
#3192=ORIENTED_EDGE('',*,*,#4551,.T.);
#3193=ORIENTED_EDGE('',*,*,#4552,.T.);
#3194=ORIENTED_EDGE('',*,*,#4434,.T.);
#3195=ORIENTED_EDGE('',*,*,#4548,.T.);
#3196=ORIENTED_EDGE('',*,*,#4435,.T.);
#3197=ORIENTED_EDGE('',*,*,#4552,.F.);
#3198=ORIENTED_EDGE('',*,*,#4553,.F.);
#3199=ORIENTED_EDGE('',*,*,#4554,.F.);
#3200=ORIENTED_EDGE('',*,*,#4466,.T.);
#3201=ORIENTED_EDGE('',*,*,#4555,.F.);
#3202=ORIENTED_EDGE('',*,*,#4465,.T.);
#3203=ORIENTED_EDGE('',*,*,#4493,.T.);
#3204=ORIENTED_EDGE('',*,*,#4412,.T.);
#3205=ORIENTED_EDGE('',*,*,#4555,.T.);
#3206=ORIENTED_EDGE('',*,*,#4447,.T.);
#3207=ORIENTED_EDGE('',*,*,#4532,.T.);
#3208=ORIENTED_EDGE('',*,*,#4556,.T.);
#3209=ORIENTED_EDGE('',*,*,#4557,.T.);
#3210=ORIENTED_EDGE('',*,*,#4558,.T.);
#3211=ORIENTED_EDGE('',*,*,#4524,.T.);
#3212=ORIENTED_EDGE('',*,*,#4559,.T.);
#3213=ORIENTED_EDGE('',*,*,#4560,.T.);
#3214=ORIENTED_EDGE('',*,*,#4561,.T.);
#3215=ORIENTED_EDGE('',*,*,#4562,.T.);
#3216=ORIENTED_EDGE('',*,*,#4563,.F.);
#3217=ORIENTED_EDGE('',*,*,#4564,.T.);
#3218=ORIENTED_EDGE('',*,*,#4451,.T.);
#3219=ORIENTED_EDGE('',*,*,#4522,.T.);
#3220=ORIENTED_EDGE('',*,*,#4565,.T.);
#3221=ORIENTED_EDGE('',*,*,#4566,.T.);
#3222=ORIENTED_EDGE('',*,*,#4452,.T.);
#3223=ORIENTED_EDGE('',*,*,#4564,.F.);
#3224=ORIENTED_EDGE('',*,*,#4567,.F.);
#3225=ORIENTED_EDGE('',*,*,#4514,.F.);
#3226=ORIENTED_EDGE('',*,*,#4512,.F.);
#3227=ORIENTED_EDGE('',*,*,#4455,.T.);
#3228=ORIENTED_EDGE('',*,*,#4510,.T.);
#3229=ORIENTED_EDGE('',*,*,#4568,.T.);
#3230=ORIENTED_EDGE('',*,*,#4569,.T.);
#3231=ORIENTED_EDGE('',*,*,#4570,.T.);
#3232=ORIENTED_EDGE('',*,*,#4502,.T.);
#3233=ORIENTED_EDGE('',*,*,#4571,.T.);
#3234=ORIENTED_EDGE('',*,*,#4572,.T.);
#3235=ORIENTED_EDGE('',*,*,#4463,.T.);
#3236=ORIENTED_EDGE('',*,*,#4499,.T.);
#3237=ORIENTED_EDGE('',*,*,#4573,.T.);
#3238=ORIENTED_EDGE('',*,*,#4574,.T.);
#3239=ORIENTED_EDGE('',*,*,#4575,.T.);
#3240=ORIENTED_EDGE('',*,*,#4490,.T.);
#3241=ORIENTED_EDGE('',*,*,#4576,.T.);
#3242=ORIENTED_EDGE('',*,*,#4577,.T.);
#3243=ORIENTED_EDGE('',*,*,#4467,.T.);
#3244=ORIENTED_EDGE('',*,*,#4554,.T.);
#3245=ORIENTED_EDGE('',*,*,#4578,.T.);
#3246=ORIENTED_EDGE('',*,*,#4579,.T.);
#3247=ORIENTED_EDGE('',*,*,#4580,.T.);
#3248=ORIENTED_EDGE('',*,*,#4546,.T.);
#3249=ORIENTED_EDGE('',*,*,#4581,.T.);
#3250=ORIENTED_EDGE('',*,*,#4582,.T.);
#3251=ORIENTED_EDGE('',*,*,#4471,.T.);
#3252=ORIENTED_EDGE('',*,*,#4543,.T.);
#3253=ORIENTED_EDGE('',*,*,#4583,.T.);
#3254=ORIENTED_EDGE('',*,*,#4584,.T.);
#3255=ORIENTED_EDGE('',*,*,#4585,.T.);
#3256=ORIENTED_EDGE('',*,*,#4535,.T.);
#3257=ORIENTED_EDGE('',*,*,#4586,.T.);
#3258=ORIENTED_EDGE('',*,*,#4587,.T.);
#3259=ORIENTED_EDGE('',*,*,#4588,.F.);
#3260=ORIENTED_EDGE('',*,*,#4589,.F.);
#3261=ORIENTED_EDGE('',*,*,#4590,.F.);
#3262=ORIENTED_EDGE('',*,*,#4591,.F.);
#3263=ORIENTED_EDGE('',*,*,#4472,.F.);
#3264=ORIENTED_EDGE('',*,*,#4473,.F.);
#3265=ORIENTED_EDGE('',*,*,#4592,.F.);
#3266=ORIENTED_EDGE('',*,*,#4593,.F.);
#3267=ORIENTED_EDGE('',*,*,#4594,.F.);
#3268=ORIENTED_EDGE('',*,*,#4595,.F.);
#3269=ORIENTED_EDGE('',*,*,#4474,.F.);
#3270=ORIENTED_EDGE('',*,*,#4477,.F.);
#3271=ORIENTED_EDGE('',*,*,#4479,.F.);
#3272=ORIENTED_EDGE('',*,*,#4478,.F.);
#3273=ORIENTED_EDGE('',*,*,#4480,.F.);
#3274=ORIENTED_EDGE('',*,*,#4596,.F.);
#3275=ORIENTED_EDGE('',*,*,#4597,.F.);
#3276=ORIENTED_EDGE('',*,*,#4598,.F.);
#3277=ORIENTED_EDGE('',*,*,#4599,.F.);
#3278=ORIENTED_EDGE('',*,*,#4482,.F.);
#3279=ORIENTED_EDGE('',*,*,#4481,.F.);
#3280=ORIENTED_EDGE('',*,*,#4483,.F.);
#3281=ORIENTED_EDGE('',*,*,#4600,.F.);
#3282=ORIENTED_EDGE('',*,*,#4601,.F.);
#3283=ORIENTED_EDGE('',*,*,#4602,.F.);
#3284=ORIENTED_EDGE('',*,*,#4603,.F.);
#3285=ORIENTED_EDGE('',*,*,#4484,.F.);
#3286=ORIENTED_EDGE('',*,*,#4487,.F.);
#3287=ORIENTED_EDGE('',*,*,#4604,.F.);
#3288=ORIENTED_EDGE('',*,*,#4605,.F.);
#3289=ORIENTED_EDGE('',*,*,#4606,.F.);
#3290=ORIENTED_EDGE('',*,*,#4607,.F.);
#3291=ORIENTED_EDGE('',*,*,#4608,.F.);
#3292=ORIENTED_EDGE('',*,*,#4609,.F.);
#3293=ORIENTED_EDGE('',*,*,#4610,.F.);
#3294=ORIENTED_EDGE('',*,*,#4611,.F.);
#3295=ORIENTED_EDGE('',*,*,#4489,.F.);
#3296=ORIENTED_EDGE('',*,*,#4488,.F.);
#3297=ORIENTED_EDGE('',*,*,#4494,.F.);
#3298=ORIENTED_EDGE('',*,*,#4491,.T.);
#3299=ORIENTED_EDGE('',*,*,#4575,.F.);
#3300=ORIENTED_EDGE('',*,*,#4612,.T.);
#3301=ORIENTED_EDGE('',*,*,#4613,.T.);
#3302=ORIENTED_EDGE('',*,*,#4496,.F.);
#3303=ORIENTED_EDGE('',*,*,#4614,.F.);
#3304=ORIENTED_EDGE('',*,*,#4615,.T.);
#3305=ORIENTED_EDGE('',*,*,#4573,.F.);
#3306=ORIENTED_EDGE('',*,*,#4498,.T.);
#3307=ORIENTED_EDGE('',*,*,#4613,.F.);
#3308=ORIENTED_EDGE('',*,*,#4616,.T.);
#3309=ORIENTED_EDGE('',*,*,#4614,.T.);
#3310=ORIENTED_EDGE('',*,*,#4495,.F.);
#3311=ORIENTED_EDGE('',*,*,#4570,.F.);
#3312=ORIENTED_EDGE('',*,*,#4617,.T.);
#3313=ORIENTED_EDGE('',*,*,#4618,.F.);
#3314=ORIENTED_EDGE('',*,*,#4505,.F.);
#3315=ORIENTED_EDGE('',*,*,#4503,.T.);
#3316=ORIENTED_EDGE('',*,*,#4619,.T.);
#3317=ORIENTED_EDGE('',*,*,#4568,.F.);
#3318=ORIENTED_EDGE('',*,*,#4509,.T.);
#3319=ORIENTED_EDGE('',*,*,#4507,.F.);
#3320=ORIENTED_EDGE('',*,*,#4620,.T.);
#3321=ORIENTED_EDGE('',*,*,#4618,.T.);
#3322=ORIENTED_EDGE('',*,*,#4621,.T.);
#3323=ORIENTED_EDGE('',*,*,#4620,.F.);
#3324=ORIENTED_EDGE('',*,*,#4506,.F.);
#3325=ORIENTED_EDGE('',*,*,#4622,.T.);
#3326=ORIENTED_EDGE('',*,*,#4516,.F.);
#3327=ORIENTED_EDGE('',*,*,#4515,.F.);
#3328=ORIENTED_EDGE('',*,*,#4521,.T.);
#3329=ORIENTED_EDGE('',*,*,#4518,.F.);
#3330=ORIENTED_EDGE('',*,*,#4623,.T.);
#3331=ORIENTED_EDGE('',*,*,#4624,.T.);
#3332=ORIENTED_EDGE('',*,*,#4561,.F.);
#3333=ORIENTED_EDGE('',*,*,#4623,.F.);
#3334=ORIENTED_EDGE('',*,*,#4517,.F.);
#3335=ORIENTED_EDGE('',*,*,#4625,.T.);
#3336=ORIENTED_EDGE('',*,*,#4626,.T.);
#3337=ORIENTED_EDGE('',*,*,#4527,.F.);
#3338=ORIENTED_EDGE('',*,*,#4525,.T.);
#3339=ORIENTED_EDGE('',*,*,#4558,.F.);
#3340=ORIENTED_EDGE('',*,*,#4627,.T.);
#3341=ORIENTED_EDGE('',*,*,#4628,.T.);
#3342=ORIENTED_EDGE('',*,*,#4629,.T.);
#3343=ORIENTED_EDGE('',*,*,#4556,.F.);
#3344=ORIENTED_EDGE('',*,*,#4531,.T.);
#3345=ORIENTED_EDGE('',*,*,#4529,.F.);
#3346=ORIENTED_EDGE('',*,*,#4630,.T.);
#3347=ORIENTED_EDGE('',*,*,#4628,.F.);
#3348=ORIENTED_EDGE('',*,*,#4631,.T.);
#3349=ORIENTED_EDGE('',*,*,#4630,.F.);
#3350=ORIENTED_EDGE('',*,*,#4528,.F.);
#3351=ORIENTED_EDGE('',*,*,#4538,.F.);
#3352=ORIENTED_EDGE('',*,*,#4536,.T.);
#3353=ORIENTED_EDGE('',*,*,#4585,.F.);
#3354=ORIENTED_EDGE('',*,*,#4632,.T.);
#3355=ORIENTED_EDGE('',*,*,#4633,.T.);
#3356=ORIENTED_EDGE('',*,*,#4634,.T.);
#3357=ORIENTED_EDGE('',*,*,#4583,.F.);
#3358=ORIENTED_EDGE('',*,*,#4542,.T.);
#3359=ORIENTED_EDGE('',*,*,#4540,.F.);
#3360=ORIENTED_EDGE('',*,*,#4635,.T.);
#3361=ORIENTED_EDGE('',*,*,#4633,.F.);
#3362=ORIENTED_EDGE('',*,*,#4636,.T.);
#3363=ORIENTED_EDGE('',*,*,#4635,.F.);
#3364=ORIENTED_EDGE('',*,*,#4539,.F.);
#3365=ORIENTED_EDGE('',*,*,#4549,.F.);
#3366=ORIENTED_EDGE('',*,*,#4547,.T.);
#3367=ORIENTED_EDGE('',*,*,#4580,.F.);
#3368=ORIENTED_EDGE('',*,*,#4637,.T.);
#3369=ORIENTED_EDGE('',*,*,#4638,.T.);
#3370=ORIENTED_EDGE('',*,*,#4639,.T.);
#3371=ORIENTED_EDGE('',*,*,#4578,.F.);
#3372=ORIENTED_EDGE('',*,*,#4553,.T.);
#3373=ORIENTED_EDGE('',*,*,#4551,.F.);
#3374=ORIENTED_EDGE('',*,*,#4640,.T.);
#3375=ORIENTED_EDGE('',*,*,#4638,.F.);
#3376=ORIENTED_EDGE('',*,*,#4641,.T.);
#3377=ORIENTED_EDGE('',*,*,#4640,.F.);
#3378=ORIENTED_EDGE('',*,*,#4550,.F.);
#3379=ORIENTED_EDGE('',*,*,#4588,.T.);
#3380=ORIENTED_EDGE('',*,*,#4642,.T.);
#3381=ORIENTED_EDGE('',*,*,#4560,.F.);
#3382=ORIENTED_EDGE('',*,*,#4643,.T.);
#3383=ORIENTED_EDGE('',*,*,#4589,.T.);
#3384=ORIENTED_EDGE('',*,*,#4642,.F.);
#3385=ORIENTED_EDGE('',*,*,#4591,.T.);
#3386=ORIENTED_EDGE('',*,*,#4590,.T.);
#3387=ORIENTED_EDGE('',*,*,#4643,.F.);
#3388=ORIENTED_EDGE('',*,*,#4559,.F.);
#3389=ORIENTED_EDGE('',*,*,#4627,.F.);
#3390=ORIENTED_EDGE('',*,*,#4557,.F.);
#3391=ORIENTED_EDGE('',*,*,#4629,.F.);
#3392=ORIENTED_EDGE('',*,*,#4631,.F.);
#3393=ORIENTED_EDGE('',*,*,#4592,.T.);
#3394=ORIENTED_EDGE('',*,*,#4644,.T.);
#3395=ORIENTED_EDGE('',*,*,#4566,.F.);
#3396=ORIENTED_EDGE('',*,*,#4645,.T.);
#3397=ORIENTED_EDGE('',*,*,#4593,.T.);
#3398=ORIENTED_EDGE('',*,*,#4644,.F.);
#3399=ORIENTED_EDGE('',*,*,#4595,.T.);
#3400=ORIENTED_EDGE('',*,*,#4594,.T.);
#3401=ORIENTED_EDGE('',*,*,#4645,.F.);
#3402=ORIENTED_EDGE('',*,*,#4565,.F.);
#3403=ORIENTED_EDGE('',*,*,#4624,.F.);
#3404=ORIENTED_EDGE('',*,*,#4626,.F.);
#3405=ORIENTED_EDGE('',*,*,#4646,.T.);
#3406=ORIENTED_EDGE('',*,*,#4562,.F.);
#3407=ORIENTED_EDGE('',*,*,#4625,.F.);
#3408=ORIENTED_EDGE('',*,*,#4622,.F.);
#3409=ORIENTED_EDGE('',*,*,#4567,.T.);
#3410=ORIENTED_EDGE('',*,*,#4563,.T.);
#3411=ORIENTED_EDGE('',*,*,#4646,.F.);
#3412=ORIENTED_EDGE('',*,*,#4599,.T.);
#3413=ORIENTED_EDGE('',*,*,#4647,.T.);
#3414=ORIENTED_EDGE('',*,*,#4572,.F.);
#3415=ORIENTED_EDGE('',*,*,#4648,.T.);
#3416=ORIENTED_EDGE('',*,*,#4596,.T.);
#3417=ORIENTED_EDGE('',*,*,#4647,.F.);
#3418=ORIENTED_EDGE('',*,*,#4598,.T.);
#3419=ORIENTED_EDGE('',*,*,#4597,.T.);
#3420=ORIENTED_EDGE('',*,*,#4648,.F.);
#3421=ORIENTED_EDGE('',*,*,#4571,.F.);
#3422=ORIENTED_EDGE('',*,*,#4621,.F.);
#3423=ORIENTED_EDGE('',*,*,#4617,.F.);
#3424=ORIENTED_EDGE('',*,*,#4569,.F.);
#3425=ORIENTED_EDGE('',*,*,#4619,.F.);
#3426=ORIENTED_EDGE('',*,*,#4603,.T.);
#3427=ORIENTED_EDGE('',*,*,#4649,.T.);
#3428=ORIENTED_EDGE('',*,*,#4577,.F.);
#3429=ORIENTED_EDGE('',*,*,#4650,.T.);
#3430=ORIENTED_EDGE('',*,*,#4600,.T.);
#3431=ORIENTED_EDGE('',*,*,#4649,.F.);
#3432=ORIENTED_EDGE('',*,*,#4602,.T.);
#3433=ORIENTED_EDGE('',*,*,#4601,.T.);
#3434=ORIENTED_EDGE('',*,*,#4650,.F.);
#3435=ORIENTED_EDGE('',*,*,#4576,.F.);
#3436=ORIENTED_EDGE('',*,*,#4612,.F.);
#3437=ORIENTED_EDGE('',*,*,#4574,.F.);
#3438=ORIENTED_EDGE('',*,*,#4615,.F.);
#3439=ORIENTED_EDGE('',*,*,#4616,.F.);
#3440=ORIENTED_EDGE('',*,*,#4607,.T.);
#3441=ORIENTED_EDGE('',*,*,#4651,.T.);
#3442=ORIENTED_EDGE('',*,*,#4582,.F.);
#3443=ORIENTED_EDGE('',*,*,#4652,.T.);
#3444=ORIENTED_EDGE('',*,*,#4604,.T.);
#3445=ORIENTED_EDGE('',*,*,#4651,.F.);
#3446=ORIENTED_EDGE('',*,*,#4606,.T.);
#3447=ORIENTED_EDGE('',*,*,#4605,.T.);
#3448=ORIENTED_EDGE('',*,*,#4652,.F.);
#3449=ORIENTED_EDGE('',*,*,#4581,.F.);
#3450=ORIENTED_EDGE('',*,*,#4637,.F.);
#3451=ORIENTED_EDGE('',*,*,#4579,.F.);
#3452=ORIENTED_EDGE('',*,*,#4639,.F.);
#3453=ORIENTED_EDGE('',*,*,#4641,.F.);
#3454=ORIENTED_EDGE('',*,*,#4608,.T.);
#3455=ORIENTED_EDGE('',*,*,#4653,.T.);
#3456=ORIENTED_EDGE('',*,*,#4587,.F.);
#3457=ORIENTED_EDGE('',*,*,#4654,.T.);
#3458=ORIENTED_EDGE('',*,*,#4609,.T.);
#3459=ORIENTED_EDGE('',*,*,#4653,.F.);
#3460=ORIENTED_EDGE('',*,*,#4611,.T.);
#3461=ORIENTED_EDGE('',*,*,#4610,.T.);
#3462=ORIENTED_EDGE('',*,*,#4654,.F.);
#3463=ORIENTED_EDGE('',*,*,#4586,.F.);
#3464=ORIENTED_EDGE('',*,*,#4632,.F.);
#3465=ORIENTED_EDGE('',*,*,#4584,.F.);
#3466=ORIENTED_EDGE('',*,*,#4634,.F.);
#3467=ORIENTED_EDGE('',*,*,#4636,.F.);
#3468=EDGE_CURVE('',#4655,#4655,#5499,.F.);
#3469=EDGE_CURVE('',#4656,#4656,#5500,.T.);
#3470=EDGE_CURVE('',#4657,#4657,#5501,.T.);
#3471=EDGE_CURVE('',#4658,#4658,#5502,.F.);
#3472=EDGE_CURVE('',#4659,#4660,#5503,.F.);
#3473=EDGE_CURVE('',#4660,#4661,#155,.F.);
#3474=EDGE_CURVE('',#4661,#4662,#5504,.F.);
#3475=EDGE_CURVE('',#4662,#4663,#156,.F.);
#3476=EDGE_CURVE('',#4663,#4664,#5505,.F.);
#3477=EDGE_CURVE('',#4664,#4665,#157,.F.);
#3478=EDGE_CURVE('',#4665,#4666,#5506,.F.);
#3479=EDGE_CURVE('',#4666,#4667,#158,.F.);
#3480=EDGE_CURVE('',#4667,#4668,#5507,.F.);
#3481=EDGE_CURVE('',#4668,#4669,#159,.F.);
#3482=EDGE_CURVE('',#4669,#4670,#5508,.F.);
#3483=EDGE_CURVE('',#4670,#4671,#160,.F.);
#3484=EDGE_CURVE('',#4671,#4672,#5509,.F.);
#3485=EDGE_CURVE('',#4672,#4673,#161,.F.);
#3486=EDGE_CURVE('',#4673,#4674,#5510,.F.);
#3487=EDGE_CURVE('',#4674,#4675,#162,.F.);
#3488=EDGE_CURVE('',#4675,#4676,#5511,.F.);
#3489=EDGE_CURVE('',#4676,#4677,#163,.F.);
#3490=EDGE_CURVE('',#4677,#4678,#5512,.F.);
#3491=EDGE_CURVE('',#4678,#4679,#164,.F.);
#3492=EDGE_CURVE('',#4679,#4680,#5513,.F.);
#3493=EDGE_CURVE('',#4680,#4681,#165,.F.);
#3494=EDGE_CURVE('',#4681,#4682,#5514,.F.);
#3495=EDGE_CURVE('',#4682,#4683,#166,.F.);
#3496=EDGE_CURVE('',#4683,#4684,#5515,.F.);
#3497=EDGE_CURVE('',#4684,#4685,#167,.F.);
#3498=EDGE_CURVE('',#4685,#4686,#5516,.F.);
#3499=EDGE_CURVE('',#4686,#4687,#168,.F.);
#3500=EDGE_CURVE('',#4687,#4688,#5517,.F.);
#3501=EDGE_CURVE('',#4688,#4689,#169,.F.);
#3502=EDGE_CURVE('',#4689,#4690,#5518,.F.);
#3503=EDGE_CURVE('',#4690,#4691,#170,.F.);
#3504=EDGE_CURVE('',#4691,#4692,#5519,.F.);
#3505=EDGE_CURVE('',#4692,#4693,#171,.F.);
#3506=EDGE_CURVE('',#4693,#4694,#5520,.F.);
#3507=EDGE_CURVE('',#4694,#4695,#172,.F.);
#3508=EDGE_CURVE('',#4695,#4696,#5521,.F.);
#3509=EDGE_CURVE('',#4696,#4697,#173,.F.);
#3510=EDGE_CURVE('',#4697,#4698,#5522,.F.);
#3511=EDGE_CURVE('',#4698,#4699,#174,.F.);
#3512=EDGE_CURVE('',#4699,#4700,#5523,.F.);
#3513=EDGE_CURVE('',#4700,#4701,#175,.F.);
#3514=EDGE_CURVE('',#4701,#4702,#5524,.F.);
#3515=EDGE_CURVE('',#4702,#4703,#176,.F.);
#3516=EDGE_CURVE('',#4703,#4704,#5525,.F.);
#3517=EDGE_CURVE('',#4704,#4705,#177,.F.);
#3518=EDGE_CURVE('',#4705,#4706,#5526,.F.);
#3519=EDGE_CURVE('',#4706,#4707,#178,.F.);
#3520=EDGE_CURVE('',#4707,#4708,#5527,.F.);
#3521=EDGE_CURVE('',#4708,#4709,#179,.F.);
#3522=EDGE_CURVE('',#4709,#4710,#5528,.F.);
#3523=EDGE_CURVE('',#4710,#4711,#180,.F.);
#3524=EDGE_CURVE('',#4711,#4712,#5529,.F.);
#3525=EDGE_CURVE('',#4712,#4713,#181,.F.);
#3526=EDGE_CURVE('',#4713,#4714,#5530,.F.);
#3527=EDGE_CURVE('',#4714,#4715,#182,.F.);
#3528=EDGE_CURVE('',#4715,#4716,#5531,.F.);
#3529=EDGE_CURVE('',#4716,#4717,#183,.F.);
#3530=EDGE_CURVE('',#4717,#4718,#5532,.F.);
#3531=EDGE_CURVE('',#4718,#4719,#184,.F.);
#3532=EDGE_CURVE('',#4719,#4720,#5533,.F.);
#3533=EDGE_CURVE('',#4720,#4721,#185,.F.);
#3534=EDGE_CURVE('',#4721,#4722,#5534,.F.);
#3535=EDGE_CURVE('',#4722,#4723,#186,.F.);
#3536=EDGE_CURVE('',#4723,#4724,#5535,.F.);
#3537=EDGE_CURVE('',#4724,#4725,#187,.F.);
#3538=EDGE_CURVE('',#4725,#4726,#5536,.F.);
#3539=EDGE_CURVE('',#4726,#4727,#188,.F.);
#3540=EDGE_CURVE('',#4727,#4728,#5537,.F.);
#3541=EDGE_CURVE('',#4728,#4729,#189,.F.);
#3542=EDGE_CURVE('',#4729,#4730,#5538,.F.);
#3543=EDGE_CURVE('',#4730,#4731,#190,.F.);
#3544=EDGE_CURVE('',#4731,#4732,#5539,.F.);
#3545=EDGE_CURVE('',#4732,#4733,#191,.F.);
#3546=EDGE_CURVE('',#4733,#4734,#5540,.F.);
#3547=EDGE_CURVE('',#4734,#4735,#192,.F.);
#3548=EDGE_CURVE('',#4735,#4736,#5541,.F.);
#3549=EDGE_CURVE('',#4736,#4737,#193,.F.);
#3550=EDGE_CURVE('',#4737,#4738,#5542,.F.);
#3551=EDGE_CURVE('',#4738,#4659,#194,.F.);
#3552=EDGE_CURVE('',#4739,#4739,#5543,.T.);
#3553=EDGE_CURVE('',#4699,#4740,#195,.T.);
#3554=EDGE_CURVE('',#4740,#4741,#5544,.T.);
#3555=EDGE_CURVE('',#4741,#4700,#196,.T.);
#3556=EDGE_CURVE('',#4741,#4742,#197,.T.);
#3557=EDGE_CURVE('',#4742,#4743,#198,.T.);
#3558=EDGE_CURVE('',#4743,#4701,#199,.T.);
#3559=EDGE_CURVE('',#4744,#4745,#5545,.T.);
#3560=EDGE_CURVE('',#4746,#4744,#200,.T.);
#3561=EDGE_CURVE('',#4702,#4746,#201,.T.);
#3562=EDGE_CURVE('',#4745,#4743,#202,.T.);
#3563=EDGE_CURVE('',#4746,#4747,#203,.T.);
#3564=EDGE_CURVE('',#4747,#4748,#204,.T.);
#3565=EDGE_CURVE('',#4748,#4703,#205,.T.);
#3566=EDGE_CURVE('',#4748,#4749,#5546,.T.);
#3567=EDGE_CURVE('',#4749,#4704,#206,.T.);
#3568=EDGE_CURVE('',#4749,#4750,#207,.T.);
#3569=EDGE_CURVE('',#4750,#4751,#208,.T.);
#3570=EDGE_CURVE('',#4751,#4705,#209,.T.);
#3571=EDGE_CURVE('',#4752,#4751,#210,.T.);
#3572=EDGE_CURVE('',#4753,#4752,#5547,.T.);
#3573=EDGE_CURVE('',#4754,#4753,#211,.T.);
#3574=EDGE_CURVE('',#4706,#4754,#212,.T.);
#3575=EDGE_CURVE('',#4754,#4755,#213,.T.);
#3576=EDGE_CURVE('',#4755,#4756,#214,.T.);
#3577=EDGE_CURVE('',#4756,#4707,#215,.T.);
#3578=EDGE_CURVE('',#4756,#4757,#5548,.T.);
#3579=EDGE_CURVE('',#4757,#4708,#216,.T.);
#3580=EDGE_CURVE('',#4757,#4758,#217,.T.);
#3581=EDGE_CURVE('',#4758,#4759,#218,.T.);
#3582=EDGE_CURVE('',#4759,#4709,#219,.T.);
#3583=EDGE_CURVE('',#4760,#4759,#220,.T.);
#3584=EDGE_CURVE('',#4761,#4760,#5549,.T.);
#3585=EDGE_CURVE('',#4762,#4761,#221,.T.);
#3586=EDGE_CURVE('',#4710,#4762,#222,.T.);
#3587=EDGE_CURVE('',#4762,#4763,#223,.T.);
#3588=EDGE_CURVE('',#4763,#4764,#224,.T.);
#3589=EDGE_CURVE('',#4764,#4711,#225,.T.);
#3590=EDGE_CURVE('',#4764,#4765,#5550,.T.);
#3591=EDGE_CURVE('',#4765,#4712,#226,.T.);
#3592=EDGE_CURVE('',#4765,#4766,#227,.T.);
#3593=EDGE_CURVE('',#4766,#4767,#228,.T.);
#3594=EDGE_CURVE('',#4767,#4713,#229,.T.);
#3595=EDGE_CURVE('',#4768,#4767,#230,.T.);
#3596=EDGE_CURVE('',#4769,#4768,#5551,.T.);
#3597=EDGE_CURVE('',#4770,#4769,#231,.T.);
#3598=EDGE_CURVE('',#4714,#4770,#232,.T.);
#3599=EDGE_CURVE('',#4770,#4771,#233,.T.);
#3600=EDGE_CURVE('',#4771,#4772,#234,.T.);
#3601=EDGE_CURVE('',#4772,#4715,#235,.T.);
#3602=EDGE_CURVE('',#4772,#4773,#5552,.T.);
#3603=EDGE_CURVE('',#4773,#4716,#236,.T.);
#3604=EDGE_CURVE('',#4773,#4774,#237,.T.);
#3605=EDGE_CURVE('',#4774,#4775,#238,.T.);
#3606=EDGE_CURVE('',#4775,#4717,#239,.T.);
#3607=EDGE_CURVE('',#4776,#4775,#240,.T.);
#3608=EDGE_CURVE('',#4777,#4776,#5553,.T.);
#3609=EDGE_CURVE('',#4778,#4777,#241,.T.);
#3610=EDGE_CURVE('',#4718,#4778,#242,.T.);
#3611=EDGE_CURVE('',#4778,#4779,#243,.T.);
#3612=EDGE_CURVE('',#4779,#4780,#244,.T.);
#3613=EDGE_CURVE('',#4780,#4719,#245,.T.);
#3614=EDGE_CURVE('',#4780,#4781,#5554,.T.);
#3615=EDGE_CURVE('',#4781,#4720,#246,.T.);
#3616=EDGE_CURVE('',#4781,#4782,#247,.T.);
#3617=EDGE_CURVE('',#4782,#4783,#248,.T.);
#3618=EDGE_CURVE('',#4783,#4721,#249,.T.);
#3619=EDGE_CURVE('',#4784,#4783,#250,.T.);
#3620=EDGE_CURVE('',#4785,#4784,#5555,.T.);
#3621=EDGE_CURVE('',#4786,#4785,#251,.T.);
#3622=EDGE_CURVE('',#4722,#4786,#252,.T.);
#3623=EDGE_CURVE('',#4786,#4787,#253,.T.);
#3624=EDGE_CURVE('',#4787,#4788,#254,.T.);
#3625=EDGE_CURVE('',#4788,#4723,#255,.T.);
#3626=EDGE_CURVE('',#4788,#4789,#5556,.T.);
#3627=EDGE_CURVE('',#4789,#4724,#256,.T.);
#3628=EDGE_CURVE('',#4789,#4790,#257,.T.);
#3629=EDGE_CURVE('',#4790,#4791,#258,.T.);
#3630=EDGE_CURVE('',#4791,#4725,#259,.T.);
#3631=EDGE_CURVE('',#4792,#4791,#260,.T.);
#3632=EDGE_CURVE('',#4793,#4792,#5557,.T.);
#3633=EDGE_CURVE('',#4794,#4793,#261,.T.);
#3634=EDGE_CURVE('',#4726,#4794,#262,.T.);
#3635=EDGE_CURVE('',#4794,#4795,#263,.T.);
#3636=EDGE_CURVE('',#4795,#4796,#264,.T.);
#3637=EDGE_CURVE('',#4796,#4727,#265,.T.);
#3638=EDGE_CURVE('',#4796,#4797,#5558,.T.);
#3639=EDGE_CURVE('',#4797,#4728,#266,.T.);
#3640=EDGE_CURVE('',#4797,#4798,#267,.T.);
#3641=EDGE_CURVE('',#4798,#4799,#268,.T.);
#3642=EDGE_CURVE('',#4799,#4729,#269,.T.);
#3643=EDGE_CURVE('',#4800,#4799,#270,.T.);
#3644=EDGE_CURVE('',#4801,#4800,#5559,.T.);
#3645=EDGE_CURVE('',#4802,#4801,#271,.T.);
#3646=EDGE_CURVE('',#4730,#4802,#272,.T.);
#3647=EDGE_CURVE('',#4802,#4803,#273,.T.);
#3648=EDGE_CURVE('',#4803,#4804,#274,.T.);
#3649=EDGE_CURVE('',#4804,#4731,#275,.T.);
#3650=EDGE_CURVE('',#4804,#4805,#5560,.T.);
#3651=EDGE_CURVE('',#4805,#4732,#276,.T.);
#3652=EDGE_CURVE('',#4805,#4806,#277,.T.);
#3653=EDGE_CURVE('',#4806,#4807,#278,.T.);
#3654=EDGE_CURVE('',#4807,#4733,#279,.T.);
#3655=EDGE_CURVE('',#4808,#4807,#280,.T.);
#3656=EDGE_CURVE('',#4809,#4808,#5561,.T.);
#3657=EDGE_CURVE('',#4810,#4809,#281,.T.);
#3658=EDGE_CURVE('',#4734,#4810,#282,.T.);
#3659=EDGE_CURVE('',#4810,#4811,#283,.T.);
#3660=EDGE_CURVE('',#4811,#4812,#284,.T.);
#3661=EDGE_CURVE('',#4812,#4735,#285,.T.);
#3662=EDGE_CURVE('',#4812,#4813,#5562,.T.);
#3663=EDGE_CURVE('',#4813,#4736,#286,.T.);
#3664=EDGE_CURVE('',#4813,#4814,#287,.T.);
#3665=EDGE_CURVE('',#4814,#4815,#288,.T.);
#3666=EDGE_CURVE('',#4815,#4737,#289,.T.);
#3667=EDGE_CURVE('',#4816,#4815,#290,.T.);
#3668=EDGE_CURVE('',#4817,#4816,#5563,.T.);
#3669=EDGE_CURVE('',#4818,#4817,#291,.T.);
#3670=EDGE_CURVE('',#4738,#4818,#292,.T.);
#3671=EDGE_CURVE('',#4818,#4819,#293,.T.);
#3672=EDGE_CURVE('',#4819,#4820,#294,.T.);
#3673=EDGE_CURVE('',#4820,#4659,#295,.T.);
#3674=EDGE_CURVE('',#4820,#4821,#5564,.T.);
#3675=EDGE_CURVE('',#4821,#4660,#296,.T.);
#3676=EDGE_CURVE('',#4821,#4822,#297,.T.);
#3677=EDGE_CURVE('',#4822,#4823,#298,.T.);
#3678=EDGE_CURVE('',#4823,#4661,#299,.T.);
#3679=EDGE_CURVE('',#4824,#4823,#300,.T.);
#3680=EDGE_CURVE('',#4825,#4824,#5565,.T.);
#3681=EDGE_CURVE('',#4826,#4825,#301,.T.);
#3682=EDGE_CURVE('',#4662,#4826,#302,.T.);
#3683=EDGE_CURVE('',#4826,#4827,#303,.T.);
#3684=EDGE_CURVE('',#4827,#4828,#304,.T.);
#3685=EDGE_CURVE('',#4828,#4663,#305,.T.);
#3686=EDGE_CURVE('',#4828,#4829,#5566,.T.);
#3687=EDGE_CURVE('',#4829,#4664,#306,.T.);
#3688=EDGE_CURVE('',#4829,#4830,#307,.T.);
#3689=EDGE_CURVE('',#4830,#4831,#308,.T.);
#3690=EDGE_CURVE('',#4831,#4665,#309,.T.);
#3691=EDGE_CURVE('',#4832,#4831,#310,.T.);
#3692=EDGE_CURVE('',#4833,#4832,#5567,.T.);
#3693=EDGE_CURVE('',#4834,#4833,#311,.T.);
#3694=EDGE_CURVE('',#4666,#4834,#312,.T.);
#3695=EDGE_CURVE('',#4834,#4835,#313,.T.);
#3696=EDGE_CURVE('',#4835,#4836,#314,.T.);
#3697=EDGE_CURVE('',#4836,#4667,#315,.T.);
#3698=EDGE_CURVE('',#4836,#4837,#5568,.T.);
#3699=EDGE_CURVE('',#4837,#4668,#316,.T.);
#3700=EDGE_CURVE('',#4837,#4838,#317,.T.);
#3701=EDGE_CURVE('',#4838,#4839,#318,.T.);
#3702=EDGE_CURVE('',#4839,#4669,#319,.T.);
#3703=EDGE_CURVE('',#4840,#4839,#320,.T.);
#3704=EDGE_CURVE('',#4841,#4840,#5569,.T.);
#3705=EDGE_CURVE('',#4842,#4841,#321,.T.);
#3706=EDGE_CURVE('',#4670,#4842,#322,.T.);
#3707=EDGE_CURVE('',#4842,#4843,#323,.T.);
#3708=EDGE_CURVE('',#4843,#4844,#324,.T.);
#3709=EDGE_CURVE('',#4844,#4671,#325,.T.);
#3710=EDGE_CURVE('',#4844,#4845,#5570,.T.);
#3711=EDGE_CURVE('',#4845,#4672,#326,.T.);
#3712=EDGE_CURVE('',#4845,#4846,#327,.T.);
#3713=EDGE_CURVE('',#4846,#4847,#328,.T.);
#3714=EDGE_CURVE('',#4847,#4673,#329,.T.);
#3715=EDGE_CURVE('',#4848,#4847,#330,.T.);
#3716=EDGE_CURVE('',#4849,#4848,#5571,.T.);
#3717=EDGE_CURVE('',#4850,#4849,#331,.T.);
#3718=EDGE_CURVE('',#4674,#4850,#332,.T.);
#3719=EDGE_CURVE('',#4850,#4851,#333,.T.);
#3720=EDGE_CURVE('',#4851,#4852,#334,.T.);
#3721=EDGE_CURVE('',#4852,#4675,#335,.T.);
#3722=EDGE_CURVE('',#4852,#4853,#5572,.T.);
#3723=EDGE_CURVE('',#4853,#4676,#336,.T.);
#3724=EDGE_CURVE('',#4853,#4854,#337,.T.);
#3725=EDGE_CURVE('',#4854,#4855,#338,.T.);
#3726=EDGE_CURVE('',#4855,#4677,#339,.T.);
#3727=EDGE_CURVE('',#4856,#4855,#340,.T.);
#3728=EDGE_CURVE('',#4857,#4856,#5573,.T.);
#3729=EDGE_CURVE('',#4858,#4857,#341,.T.);
#3730=EDGE_CURVE('',#4678,#4858,#342,.T.);
#3731=EDGE_CURVE('',#4858,#4859,#343,.T.);
#3732=EDGE_CURVE('',#4859,#4860,#344,.T.);
#3733=EDGE_CURVE('',#4860,#4679,#345,.T.);
#3734=EDGE_CURVE('',#4860,#4861,#5574,.T.);
#3735=EDGE_CURVE('',#4861,#4680,#346,.T.);
#3736=EDGE_CURVE('',#4861,#4862,#347,.T.);
#3737=EDGE_CURVE('',#4862,#4863,#348,.T.);
#3738=EDGE_CURVE('',#4863,#4681,#349,.T.);
#3739=EDGE_CURVE('',#4864,#4863,#350,.T.);
#3740=EDGE_CURVE('',#4865,#4864,#5575,.T.);
#3741=EDGE_CURVE('',#4866,#4865,#351,.T.);
#3742=EDGE_CURVE('',#4682,#4866,#352,.T.);
#3743=EDGE_CURVE('',#4866,#4867,#353,.T.);
#3744=EDGE_CURVE('',#4867,#4868,#354,.T.);
#3745=EDGE_CURVE('',#4868,#4683,#355,.T.);
#3746=EDGE_CURVE('',#4868,#4869,#5576,.T.);
#3747=EDGE_CURVE('',#4869,#4684,#356,.T.);
#3748=EDGE_CURVE('',#4869,#4870,#357,.T.);
#3749=EDGE_CURVE('',#4870,#4871,#358,.T.);
#3750=EDGE_CURVE('',#4871,#4685,#359,.T.);
#3751=EDGE_CURVE('',#4872,#4871,#360,.T.);
#3752=EDGE_CURVE('',#4873,#4872,#5577,.T.);
#3753=EDGE_CURVE('',#4874,#4873,#361,.T.);
#3754=EDGE_CURVE('',#4686,#4874,#362,.T.);
#3755=EDGE_CURVE('',#4874,#4875,#363,.T.);
#3756=EDGE_CURVE('',#4875,#4876,#364,.T.);
#3757=EDGE_CURVE('',#4876,#4687,#365,.T.);
#3758=EDGE_CURVE('',#4876,#4877,#5578,.T.);
#3759=EDGE_CURVE('',#4877,#4688,#366,.T.);
#3760=EDGE_CURVE('',#4877,#4878,#367,.T.);
#3761=EDGE_CURVE('',#4878,#4879,#368,.T.);
#3762=EDGE_CURVE('',#4879,#4689,#369,.T.);
#3763=EDGE_CURVE('',#4880,#4879,#370,.T.);
#3764=EDGE_CURVE('',#4881,#4880,#5579,.T.);
#3765=EDGE_CURVE('',#4882,#4881,#371,.T.);
#3766=EDGE_CURVE('',#4690,#4882,#372,.T.);
#3767=EDGE_CURVE('',#4882,#4883,#373,.T.);
#3768=EDGE_CURVE('',#4883,#4884,#374,.T.);
#3769=EDGE_CURVE('',#4884,#4691,#375,.T.);
#3770=EDGE_CURVE('',#4884,#4885,#5580,.T.);
#3771=EDGE_CURVE('',#4885,#4692,#376,.T.);
#3772=EDGE_CURVE('',#4885,#4886,#377,.T.);
#3773=EDGE_CURVE('',#4886,#4887,#378,.T.);
#3774=EDGE_CURVE('',#4887,#4693,#379,.T.);
#3775=EDGE_CURVE('',#4888,#4887,#380,.T.);
#3776=EDGE_CURVE('',#4889,#4888,#5581,.T.);
#3777=EDGE_CURVE('',#4890,#4889,#381,.T.);
#3778=EDGE_CURVE('',#4694,#4890,#382,.T.);
#3779=EDGE_CURVE('',#4890,#4891,#383,.T.);
#3780=EDGE_CURVE('',#4891,#4892,#384,.T.);
#3781=EDGE_CURVE('',#4892,#4695,#385,.T.);
#3782=EDGE_CURVE('',#4892,#4893,#5582,.T.);
#3783=EDGE_CURVE('',#4893,#4696,#386,.T.);
#3784=EDGE_CURVE('',#4893,#4894,#387,.T.);
#3785=EDGE_CURVE('',#4894,#4895,#388,.T.);
#3786=EDGE_CURVE('',#4895,#4697,#389,.T.);
#3787=EDGE_CURVE('',#4896,#4895,#390,.T.);
#3788=EDGE_CURVE('',#4897,#4896,#5583,.T.);
#3789=EDGE_CURVE('',#4898,#4897,#391,.T.);
#3790=EDGE_CURVE('',#4698,#4898,#392,.T.);
#3791=EDGE_CURVE('',#4898,#4899,#393,.T.);
#3792=EDGE_CURVE('',#4899,#4740,#394,.T.);
#3793=EDGE_CURVE('',#4900,#4900,#5584,.F.);
#3794=EDGE_CURVE('',#4899,#4742,#5585,.T.);
#3795=EDGE_CURVE('',#4745,#4901,#395,.T.);
#3796=EDGE_CURVE('',#4901,#4742,#396,.T.);
#3797=EDGE_CURVE('',#4902,#4744,#397,.T.);
#3798=EDGE_CURVE('',#4747,#4902,#398,.T.);
#3799=EDGE_CURVE('',#4824,#4903,#399,.T.);
#3800=EDGE_CURVE('',#4903,#4904,#5586,.T.);
#3801=EDGE_CURVE('',#4904,#4817,#400,.F.);
#3802=EDGE_CURVE('',#4816,#4905,#401,.F.);
#3803=EDGE_CURVE('',#4905,#4906,#5587,.T.);
#3804=EDGE_CURVE('',#4906,#4809,#402,.F.);
#3805=EDGE_CURVE('',#4808,#4907,#403,.F.);
#3806=EDGE_CURVE('',#4907,#4908,#5588,.T.);
#3807=EDGE_CURVE('',#4908,#4801,#404,.F.);
#3808=EDGE_CURVE('',#4800,#4909,#405,.F.);
#3809=EDGE_CURVE('',#4909,#4910,#5589,.T.);
#3810=EDGE_CURVE('',#4910,#4793,#406,.F.);
#3811=EDGE_CURVE('',#4792,#4911,#407,.F.);
#3812=EDGE_CURVE('',#4911,#4912,#5590,.T.);
#3813=EDGE_CURVE('',#4912,#4785,#408,.F.);
#3814=EDGE_CURVE('',#4784,#4913,#409,.F.);
#3815=EDGE_CURVE('',#4913,#4914,#5591,.T.);
#3816=EDGE_CURVE('',#4914,#4777,#410,.F.);
#3817=EDGE_CURVE('',#4776,#4915,#411,.F.);
#3818=EDGE_CURVE('',#4915,#4916,#5592,.T.);
#3819=EDGE_CURVE('',#4916,#4769,#412,.F.);
#3820=EDGE_CURVE('',#4768,#4917,#413,.F.);
#3821=EDGE_CURVE('',#4917,#4918,#5593,.T.);
#3822=EDGE_CURVE('',#4918,#4761,#414,.F.);
#3823=EDGE_CURVE('',#4760,#4919,#415,.F.);
#3824=EDGE_CURVE('',#4919,#4920,#5594,.T.);
#3825=EDGE_CURVE('',#4920,#4753,#416,.F.);
#3826=EDGE_CURVE('',#4752,#4921,#417,.F.);
#3827=EDGE_CURVE('',#4921,#4902,#5595,.T.);
#3828=EDGE_CURVE('',#4901,#4922,#5596,.T.);
#3829=EDGE_CURVE('',#4922,#4897,#418,.F.);
#3830=EDGE_CURVE('',#4896,#4923,#419,.F.);
#3831=EDGE_CURVE('',#4923,#4924,#5597,.T.);
#3832=EDGE_CURVE('',#4924,#4889,#420,.F.);
#3833=EDGE_CURVE('',#4888,#4925,#421,.F.);
#3834=EDGE_CURVE('',#4925,#4926,#5598,.T.);
#3835=EDGE_CURVE('',#4926,#4881,#422,.F.);
#3836=EDGE_CURVE('',#4880,#4927,#423,.F.);
#3837=EDGE_CURVE('',#4927,#4928,#5599,.T.);
#3838=EDGE_CURVE('',#4928,#4873,#424,.F.);
#3839=EDGE_CURVE('',#4872,#4929,#425,.F.);
#3840=EDGE_CURVE('',#4929,#4930,#5600,.T.);
#3841=EDGE_CURVE('',#4930,#4865,#426,.F.);
#3842=EDGE_CURVE('',#4864,#4931,#427,.F.);
#3843=EDGE_CURVE('',#4931,#4932,#5601,.T.);
#3844=EDGE_CURVE('',#4932,#4857,#428,.F.);
#3845=EDGE_CURVE('',#4856,#4933,#429,.F.);
#3846=EDGE_CURVE('',#4933,#4934,#5602,.T.);
#3847=EDGE_CURVE('',#4934,#4849,#430,.F.);
#3848=EDGE_CURVE('',#4848,#4935,#431,.F.);
#3849=EDGE_CURVE('',#4935,#4936,#5603,.T.);
#3850=EDGE_CURVE('',#4936,#4841,#432,.F.);
#3851=EDGE_CURVE('',#4840,#4937,#433,.F.);
#3852=EDGE_CURVE('',#4937,#4938,#5604,.T.);
#3853=EDGE_CURVE('',#4938,#4833,#434,.F.);
#3854=EDGE_CURVE('',#4832,#4939,#435,.F.);
#3855=EDGE_CURVE('',#4939,#4940,#5605,.T.);
#3856=EDGE_CURVE('',#4940,#4825,#436,.F.);
#3857=EDGE_CURVE('',#4941,#4941,#5606,.F.);
#3858=EDGE_CURVE('',#4747,#4750,#5607,.T.);
#3859=EDGE_CURVE('',#4921,#4750,#437,.T.);
#3860=EDGE_CURVE('',#4755,#4920,#438,.T.);
#3861=EDGE_CURVE('',#4755,#4758,#5608,.T.);
#3862=EDGE_CURVE('',#4919,#4758,#439,.T.);
#3863=EDGE_CURVE('',#4763,#4918,#440,.T.);
#3864=EDGE_CURVE('',#4763,#4766,#5609,.T.);
#3865=EDGE_CURVE('',#4917,#4766,#441,.T.);
#3866=EDGE_CURVE('',#4771,#4916,#442,.T.);
#3867=EDGE_CURVE('',#4771,#4774,#5610,.T.);
#3868=EDGE_CURVE('',#4915,#4774,#443,.T.);
#3869=EDGE_CURVE('',#4779,#4914,#444,.T.);
#3870=EDGE_CURVE('',#4779,#4782,#5611,.T.);
#3871=EDGE_CURVE('',#4913,#4782,#445,.T.);
#3872=EDGE_CURVE('',#4787,#4912,#446,.T.);
#3873=EDGE_CURVE('',#4787,#4790,#5612,.T.);
#3874=EDGE_CURVE('',#4911,#4790,#447,.T.);
#3875=EDGE_CURVE('',#4795,#4910,#448,.T.);
#3876=EDGE_CURVE('',#4795,#4798,#5613,.T.);
#3877=EDGE_CURVE('',#4909,#4798,#449,.T.);
#3878=EDGE_CURVE('',#4803,#4908,#450,.T.);
#3879=EDGE_CURVE('',#4803,#4806,#5614,.T.);
#3880=EDGE_CURVE('',#4907,#4806,#451,.T.);
#3881=EDGE_CURVE('',#4811,#4906,#452,.T.);
#3882=EDGE_CURVE('',#4811,#4814,#5615,.T.);
#3883=EDGE_CURVE('',#4905,#4814,#453,.T.);
#3884=EDGE_CURVE('',#4819,#4904,#454,.T.);
#3885=EDGE_CURVE('',#4819,#4822,#5616,.T.);
#3886=EDGE_CURVE('',#4903,#4822,#455,.T.);
#3887=EDGE_CURVE('',#4827,#4940,#456,.T.);
#3888=EDGE_CURVE('',#4827,#4830,#5617,.T.);
#3889=EDGE_CURVE('',#4939,#4830,#457,.T.);
#3890=EDGE_CURVE('',#4835,#4938,#458,.T.);
#3891=EDGE_CURVE('',#4835,#4838,#5618,.T.);
#3892=EDGE_CURVE('',#4937,#4838,#459,.T.);
#3893=EDGE_CURVE('',#4843,#4936,#460,.T.);
#3894=EDGE_CURVE('',#4843,#4846,#5619,.T.);
#3895=EDGE_CURVE('',#4935,#4846,#461,.T.);
#3896=EDGE_CURVE('',#4851,#4934,#462,.T.);
#3897=EDGE_CURVE('',#4851,#4854,#5620,.T.);
#3898=EDGE_CURVE('',#4933,#4854,#463,.T.);
#3899=EDGE_CURVE('',#4859,#4932,#464,.T.);
#3900=EDGE_CURVE('',#4859,#4862,#5621,.T.);
#3901=EDGE_CURVE('',#4931,#4862,#465,.T.);
#3902=EDGE_CURVE('',#4867,#4930,#466,.T.);
#3903=EDGE_CURVE('',#4867,#4870,#5622,.T.);
#3904=EDGE_CURVE('',#4929,#4870,#467,.T.);
#3905=EDGE_CURVE('',#4875,#4928,#468,.T.);
#3906=EDGE_CURVE('',#4875,#4878,#5623,.T.);
#3907=EDGE_CURVE('',#4927,#4878,#469,.T.);
#3908=EDGE_CURVE('',#4883,#4926,#470,.T.);
#3909=EDGE_CURVE('',#4883,#4886,#5624,.T.);
#3910=EDGE_CURVE('',#4925,#4886,#471,.T.);
#3911=EDGE_CURVE('',#4891,#4924,#472,.T.);
#3912=EDGE_CURVE('',#4891,#4894,#5625,.T.);
#3913=EDGE_CURVE('',#4923,#4894,#473,.T.);
#3914=EDGE_CURVE('',#4899,#4922,#474,.T.);
#3915=EDGE_CURVE('',#4942,#4942,#5626,.T.);
#3916=EDGE_CURVE('',#4943,#4943,#5627,.T.);
#3917=EDGE_CURVE('',#4944,#4944,#5628,.F.);
#3918=EDGE_CURVE('',#4945,#4945,#5629,.F.);
#3919=EDGE_CURVE('',#4946,#4946,#5630,.T.);
#3920=EDGE_CURVE('',#4947,#4947,#5631,.F.);
#3921=EDGE_CURVE('',#4948,#4948,#5632,.T.);
#3922=EDGE_CURVE('',#4949,#4950,#5633,.T.);
#3923=EDGE_CURVE('',#4950,#4949,#475,.T.);
#3924=EDGE_CURVE('',#4951,#4951,#5634,.F.);
#3925=EDGE_CURVE('',#4952,#4953,#476,.F.);
#3926=EDGE_CURVE('',#4953,#4952,#5635,.F.);
#3927=EDGE_CURVE('',#4954,#4955,#477,.T.);
#3928=EDGE_CURVE('',#4955,#4954,#5636,.T.);
#3929=EDGE_CURVE('',#4956,#4956,#5637,.T.);
#3930=EDGE_CURVE('',#4957,#4958,#478,.F.);
#3931=EDGE_CURVE('',#4958,#4957,#5638,.F.);
#3932=EDGE_CURVE('',#4959,#4960,#5639,.F.);
#3933=EDGE_CURVE('',#4960,#4959,#479,.T.);
#3934=EDGE_CURVE('',#4961,#4957,#480,.T.);
#3935=EDGE_CURVE('',#4962,#4961,#481,.T.);
#3936=EDGE_CURVE('',#4958,#4962,#482,.T.);
#3937=EDGE_CURVE('',#4961,#4962,#5640,.T.);
#3938=EDGE_CURVE('',#4963,#4964,#483,.F.);
#3939=EDGE_CURVE('',#4964,#4963,#5641,.T.);
#3940=EDGE_CURVE('',#4965,#4966,#5642,.F.);
#3941=EDGE_CURVE('',#4966,#4965,#484,.F.);
#3942=EDGE_CURVE('',#4964,#4967,#485,.T.);
#3943=EDGE_CURVE('',#4967,#4968,#5643,.F.);
#3944=EDGE_CURVE('',#4968,#4963,#486,.T.);
#3945=EDGE_CURVE('',#4968,#4967,#487,.T.);
#3946=EDGE_CURVE('',#4966,#4969,#488,.T.);
#3947=EDGE_CURVE('',#4969,#4970,#489,.T.);
#3948=EDGE_CURVE('',#4970,#4965,#490,.T.);
#3949=EDGE_CURVE('',#4970,#4969,#5644,.T.);
#3950=EDGE_CURVE('',#4971,#4971,#5645,.F.);
#3951=EDGE_CURVE('',#4972,#4972,#5646,.T.);
#3952=EDGE_CURVE('',#4973,#4973,#5647,.F.);
#3953=EDGE_CURVE('',#4974,#4974,#5648,.T.);
#3954=EDGE_CURVE('',#4975,#4976,#5649,.T.);
#3955=EDGE_CURVE('',#4976,#4975,#491,.T.);
#3956=EDGE_CURVE('',#4977,#4977,#5650,.F.);
#3957=EDGE_CURVE('',#4978,#4979,#492,.F.);
#3958=EDGE_CURVE('',#4979,#4978,#5651,.F.);
#3959=EDGE_CURVE('',#4980,#4981,#493,.T.);
#3960=EDGE_CURVE('',#4981,#4980,#5652,.T.);
#3961=EDGE_CURVE('',#4982,#4982,#5653,.T.);
#3962=EDGE_CURVE('',#4983,#4984,#494,.F.);
#3963=EDGE_CURVE('',#4984,#4983,#5654,.F.);
#3964=EDGE_CURVE('',#4985,#4986,#5655,.F.);
#3965=EDGE_CURVE('',#4986,#4985,#495,.T.);
#3966=EDGE_CURVE('',#4987,#4983,#496,.T.);
#3967=EDGE_CURVE('',#4988,#4987,#497,.T.);
#3968=EDGE_CURVE('',#4984,#4988,#498,.T.);
#3969=EDGE_CURVE('',#4987,#4988,#5656,.T.);
#3970=EDGE_CURVE('',#4989,#4990,#499,.F.);
#3971=EDGE_CURVE('',#4990,#4989,#5657,.T.);
#3972=EDGE_CURVE('',#4991,#4992,#5658,.F.);
#3973=EDGE_CURVE('',#4992,#4991,#500,.F.);
#3974=EDGE_CURVE('',#4990,#4993,#501,.T.);
#3975=EDGE_CURVE('',#4993,#4994,#5659,.F.);
#3976=EDGE_CURVE('',#4994,#4989,#502,.T.);
#3977=EDGE_CURVE('',#4994,#4993,#503,.T.);
#3978=EDGE_CURVE('',#4992,#4995,#504,.T.);
#3979=EDGE_CURVE('',#4995,#4996,#505,.T.);
#3980=EDGE_CURVE('',#4996,#4991,#506,.T.);
#3981=EDGE_CURVE('',#4996,#4995,#5660,.T.);
#3982=EDGE_CURVE('',#4997,#4998,#507,.T.);
#3983=EDGE_CURVE('',#4998,#4997,#5661,.T.);
#3984=EDGE_CURVE('',#4999,#4999,#5662,.F.);
#3985=EDGE_CURVE('',#5000,#5000,#5663,.F.);
#3986=EDGE_CURVE('',#5001,#5002,#508,.F.);
#3987=EDGE_CURVE('',#5002,#5001,#5664,.T.);
#3988=EDGE_CURVE('',#5003,#5004,#509,.F.);
#3989=EDGE_CURVE('',#5004,#5003,#5665,.T.);
#3990=EDGE_CURVE('',#5005,#5005,#5666,.T.);
#3991=EDGE_CURVE('',#5004,#5006,#510,.T.);
#3992=EDGE_CURVE('',#5006,#5007,#511,.T.);
#3993=EDGE_CURVE('',#5007,#5003,#512,.T.);
#3994=EDGE_CURVE('',#5007,#5006,#5667,.F.);
#3995=EDGE_CURVE('',#5008,#5008,#5668,.T.);
#3996=EDGE_CURVE('',#5009,#5009,#5669,.F.);
#3997=EDGE_CURVE('',#5010,#5011,#513,.F.);
#3998=EDGE_CURVE('',#5011,#5010,#5670,.F.);
#3999=EDGE_CURVE('',#5012,#5013,#5671,.F.);
#4000=EDGE_CURVE('',#5013,#5012,#5672,.F.);
#4001=EDGE_CURVE('',#5014,#5010,#514,.T.);
#4002=EDGE_CURVE('',#5011,#5015,#515,.T.);
#4003=EDGE_CURVE('',#5015,#5014,#516,.T.);
#4004=EDGE_CURVE('',#5014,#5015,#5673,.T.);
#4005=EDGE_CURVE('',#5016,#5012,#517,.T.);
#4006=EDGE_CURVE('',#5013,#5017,#518,.T.);
#4007=EDGE_CURVE('',#5017,#5016,#519,.T.);
#4008=EDGE_CURVE('',#5016,#5017,#5674,.F.);
#4009=EDGE_CURVE('',#5018,#5018,#5675,.T.);
#4010=EDGE_CURVE('',#5019,#5020,#520,.F.);
#4011=EDGE_CURVE('',#5020,#5019,#5676,.T.);
#4012=EDGE_CURVE('',#5021,#5022,#5677,.T.);
#4013=EDGE_CURVE('',#5022,#5021,#5678,.T.);
#4014=EDGE_CURVE('',#5022,#5019,#521,.T.);
#4015=EDGE_CURVE('',#5020,#5021,#522,.T.);
#4016=EDGE_CURVE('',#5023,#5024,#523,.T.);
#4017=EDGE_CURVE('',#5024,#5023,#5679,.T.);
#4018=EDGE_CURVE('',#5025,#5025,#5680,.F.);
#4019=EDGE_CURVE('',#5026,#5026,#5681,.F.);
#4020=EDGE_CURVE('',#5027,#5028,#524,.F.);
#4021=EDGE_CURVE('',#5028,#5027,#5682,.T.);
#4022=EDGE_CURVE('',#5029,#5030,#525,.F.);
#4023=EDGE_CURVE('',#5030,#5029,#5683,.T.);
#4024=EDGE_CURVE('',#5031,#5031,#5684,.T.);
#4025=EDGE_CURVE('',#5030,#5032,#526,.T.);
#4026=EDGE_CURVE('',#5032,#5033,#527,.T.);
#4027=EDGE_CURVE('',#5033,#5029,#528,.T.);
#4028=EDGE_CURVE('',#5033,#5032,#5685,.F.);
#4029=EDGE_CURVE('',#5034,#5034,#5686,.T.);
#4030=EDGE_CURVE('',#5035,#5035,#5687,.F.);
#4031=EDGE_CURVE('',#5036,#5037,#529,.F.);
#4032=EDGE_CURVE('',#5037,#5036,#5688,.F.);
#4033=EDGE_CURVE('',#5038,#5039,#5689,.F.);
#4034=EDGE_CURVE('',#5039,#5038,#5690,.F.);
#4035=EDGE_CURVE('',#5040,#5036,#530,.T.);
#4036=EDGE_CURVE('',#5037,#5041,#531,.T.);
#4037=EDGE_CURVE('',#5041,#5040,#532,.T.);
#4038=EDGE_CURVE('',#5040,#5041,#5691,.T.);
#4039=EDGE_CURVE('',#5042,#5038,#533,.T.);
#4040=EDGE_CURVE('',#5039,#5043,#534,.T.);
#4041=EDGE_CURVE('',#5043,#5042,#535,.T.);
#4042=EDGE_CURVE('',#5042,#5043,#5692,.F.);
#4043=EDGE_CURVE('',#5044,#5044,#5693,.T.);
#4044=EDGE_CURVE('',#5045,#5046,#536,.F.);
#4045=EDGE_CURVE('',#5046,#5045,#5694,.T.);
#4046=EDGE_CURVE('',#5047,#5048,#5695,.T.);
#4047=EDGE_CURVE('',#5048,#5047,#5696,.T.);
#4048=EDGE_CURVE('',#5048,#5045,#537,.T.);
#4049=EDGE_CURVE('',#5046,#5047,#538,.T.);
#4050=EDGE_CURVE('',#5049,#5049,#5697,.F.);
#4051=EDGE_CURVE('',#5050,#5050,#5698,.T.);
#4052=EDGE_CURVE('',#5051,#5051,#5699,.F.);
#4053=EDGE_CURVE('',#5052,#5052,#5700,.T.);
#4054=EDGE_CURVE('',#5053,#5053,#5701,.T.);
#4055=EDGE_CURVE('',#5054,#5054,#5702,.F.);
#4056=EDGE_CURVE('',#5055,#5055,#5703,.T.);
#4057=EDGE_CURVE('',#5056,#5056,#5704,.F.);
#4058=EDGE_CURVE('',#5057,#5057,#5705,.F.);
#4059=EDGE_CURVE('',#5058,#5058,#5706,.T.);
#4060=EDGE_CURVE('',#5059,#5059,#5707,.F.);
#4061=EDGE_CURVE('',#5060,#5060,#5708,.T.);
#4062=EDGE_CURVE('',#5061,#5061,#5709,.T.);
#4063=EDGE_CURVE('',#5062,#5062,#5710,.F.);
#4064=EDGE_CURVE('',#5063,#5063,#5711,.T.);
#4065=EDGE_CURVE('',#5064,#5064,#5712,.F.);
#4066=EDGE_CURVE('',#5065,#5065,#5713,.F.);
#4067=EDGE_CURVE('',#5066,#5066,#5714,.T.);
#4068=EDGE_CURVE('',#5067,#5067,#5715,.F.);
#4069=EDGE_CURVE('',#5068,#5068,#5716,.T.);
#4070=EDGE_CURVE('',#5069,#5069,#5717,.T.);
#4071=EDGE_CURVE('',#5070,#5070,#5718,.F.);
#4072=EDGE_CURVE('',#5071,#5071,#5719,.T.);
#4073=EDGE_CURVE('',#5072,#5072,#5720,.F.);
#4074=EDGE_CURVE('',#5073,#5073,#5721,.F.);
#4075=EDGE_CURVE('',#5074,#5074,#5722,.T.);
#4076=EDGE_CURVE('',#5075,#5075,#5723,.F.);
#4077=EDGE_CURVE('',#5076,#5076,#5724,.F.);
#4078=EDGE_CURVE('',#5077,#5077,#5725,.T.);
#4079=EDGE_CURVE('',#5078,#5078,#5726,.T.);
#4080=EDGE_CURVE('',#5079,#5079,#5727,.T.);
#4081=EDGE_CURVE('',#5080,#5080,#5728,.F.);
#4082=EDGE_CURVE('',#5081,#5081,#5729,.F.);
#4083=EDGE_CURVE('',#5082,#5082,#5730,.F.);
#4084=EDGE_CURVE('',#5083,#5083,#5731,.F.);
#4085=EDGE_CURVE('',#5084,#5084,#5732,.T.);
#4086=EDGE_CURVE('',#5085,#5085,#5733,.T.);
#4087=EDGE_CURVE('',#5086,#5086,#5734,.T.);
#4088=EDGE_CURVE('',#5087,#5087,#5735,.T.);
#4089=EDGE_CURVE('',#5088,#5088,#5736,.T.);
#4090=EDGE_CURVE('',#5089,#5089,#5737,.T.);
#4091=EDGE_CURVE('',#5090,#5090,#5738,.T.);
#4092=EDGE_CURVE('',#5091,#5091,#5739,.T.);
#4093=EDGE_CURVE('',#5092,#5092,#5740,.T.);
#4094=EDGE_CURVE('',#5093,#5093,#5741,.T.);
#4095=EDGE_CURVE('',#5094,#5094,#5742,.T.);
#4096=EDGE_CURVE('',#5095,#5095,#5743,.T.);
#4097=EDGE_CURVE('',#5096,#5096,#5744,.T.);
#4098=EDGE_CURVE('',#5097,#5097,#5745,.T.);
#4099=EDGE_CURVE('',#5098,#5098,#5746,.T.);
#4100=EDGE_CURVE('',#5099,#5099,#5747,.T.);
#4101=EDGE_CURVE('',#5100,#5100,#5748,.T.);
#4102=EDGE_CURVE('',#5101,#5101,#5749,.T.);
#4103=EDGE_CURVE('',#5102,#5102,#5750,.T.);
#4104=EDGE_CURVE('',#5103,#5103,#5751,.T.);
#4105=EDGE_CURVE('',#5104,#5104,#5752,.T.);
#4106=EDGE_CURVE('',#5105,#5105,#5753,.T.);
#4107=EDGE_CURVE('',#5106,#5106,#5754,.T.);
#4108=EDGE_CURVE('',#5107,#5107,#5755,.T.);
#4109=EDGE_CURVE('',#5108,#5108,#5756,.T.);
#4110=EDGE_CURVE('',#5109,#5109,#5757,.T.);
#4111=EDGE_CURVE('',#5110,#5110,#5758,.T.);
#4112=EDGE_CURVE('',#5111,#5111,#5759,.T.);
#4113=EDGE_CURVE('',#5112,#5112,#5760,.T.);
#4114=EDGE_CURVE('',#5113,#5113,#5761,.T.);
#4115=EDGE_CURVE('',#5114,#5114,#5762,.T.);
#4116=EDGE_CURVE('',#5115,#5115,#5763,.T.);
#4117=EDGE_CURVE('',#5116,#5116,#5764,.T.);
#4118=EDGE_CURVE('',#5117,#5117,#5765,.T.);
#4119=EDGE_CURVE('',#5118,#5118,#5766,.T.);
#4120=EDGE_CURVE('',#5119,#5119,#5767,.T.);
#4121=EDGE_CURVE('',#5120,#5120,#5768,.T.);
#4122=EDGE_CURVE('',#5121,#5122,#5769,.T.);
#4123=EDGE_CURVE('',#5122,#5121,#539,.T.);
#4124=EDGE_CURVE('',#5123,#5124,#5770,.T.);
#4125=EDGE_CURVE('',#5124,#5123,#540,.F.);
#4126=EDGE_CURVE('',#5125,#5125,#5771,.T.);
#4127=EDGE_CURVE('',#5126,#5126,#5772,.T.);
#4128=EDGE_CURVE('',#5127,#5128,#541,.F.);
#4129=EDGE_CURVE('',#5128,#5127,#5773,.F.);
#4130=EDGE_CURVE('',#5129,#5130,#5774,.T.);
#4131=EDGE_CURVE('',#5130,#5129,#542,.F.);
#4132=EDGE_CURVE('',#5131,#5132,#543,.F.);
#4133=EDGE_CURVE('',#5132,#5131,#544,.F.);
#4134=EDGE_CURVE('',#5133,#5133,#5775,.T.);
#4135=EDGE_CURVE('',#5134,#5135,#545,.F.);
#4136=EDGE_CURVE('',#5135,#5134,#5776,.T.);
#4137=EDGE_CURVE('',#5136,#5136,#5777,.F.);
#4138=EDGE_CURVE('',#5137,#5135,#546,.T.);
#4139=EDGE_CURVE('',#5138,#5137,#5778,.T.);
#4140=EDGE_CURVE('',#5134,#5138,#547,.T.);
#4141=EDGE_CURVE('',#5137,#5138,#548,.T.);
#4142=EDGE_CURVE('',#5139,#5140,#5779,.T.);
#4143=EDGE_CURVE('',#5140,#5139,#549,.F.);
#4144=EDGE_CURVE('',#5141,#5142,#550,.F.);
#4145=EDGE_CURVE('',#5142,#5143,#551,.F.);
#4146=EDGE_CURVE('',#5143,#5144,#552,.F.);
#4147=EDGE_CURVE('',#5144,#5145,#553,.F.);
#4148=EDGE_CURVE('',#5145,#5146,#554,.F.);
#4149=EDGE_CURVE('',#5146,#5147,#555,.F.);
#4150=EDGE_CURVE('',#5147,#5148,#556,.F.);
#4151=EDGE_CURVE('',#5148,#5149,#557,.F.);
#4152=EDGE_CURVE('',#5149,#5150,#558,.F.);
#4153=EDGE_CURVE('',#5150,#5151,#559,.F.);
#4154=EDGE_CURVE('',#5151,#5152,#560,.F.);
#4155=EDGE_CURVE('',#5152,#5153,#561,.F.);
#4156=EDGE_CURVE('',#5153,#5154,#562,.F.);
#4157=EDGE_CURVE('',#5154,#5155,#5780,.F.);
#4158=EDGE_CURVE('',#5155,#5156,#563,.F.);
#4159=EDGE_CURVE('',#5156,#5157,#564,.F.);
#4160=EDGE_CURVE('',#5157,#5158,#565,.F.);
#4161=EDGE_CURVE('',#5158,#5159,#566,.F.);
#4162=EDGE_CURVE('',#5159,#5160,#567,.F.);
#4163=EDGE_CURVE('',#5160,#5161,#568,.F.);
#4164=EDGE_CURVE('',#5161,#5162,#5781,.F.);
#4165=EDGE_CURVE('',#5162,#5163,#569,.F.);
#4166=EDGE_CURVE('',#5163,#5164,#570,.F.);
#4167=EDGE_CURVE('',#5164,#5165,#571,.F.);
#4168=EDGE_CURVE('',#5165,#5166,#572,.F.);
#4169=EDGE_CURVE('',#5166,#5141,#573,.F.);
#4170=EDGE_CURVE('',#5167,#5167,#5782,.F.);
#4171=EDGE_CURVE('',#5168,#5169,#5783,.T.);
#4172=EDGE_CURVE('',#5156,#5168,#574,.F.);
#4173=EDGE_CURVE('',#5169,#5154,#575,.F.);
#4174=EDGE_CURVE('',#5170,#5168,#576,.T.);
#4175=EDGE_CURVE('',#5157,#5170,#577,.T.);
#4176=EDGE_CURVE('',#5171,#5170,#5784,.F.);
#4177=EDGE_CURVE('',#5158,#5171,#578,.F.);
#4178=EDGE_CURVE('',#5172,#5171,#579,.T.);
#4179=EDGE_CURVE('',#5159,#5172,#580,.T.);
#4180=EDGE_CURVE('',#5173,#5172,#581,.T.);
#4181=EDGE_CURVE('',#5160,#5173,#582,.F.);
#4182=EDGE_CURVE('',#5174,#5173,#583,.T.);
#4183=EDGE_CURVE('',#5161,#5174,#584,.T.);
#4184=EDGE_CURVE('',#5175,#5174,#5785,.F.);
#4185=EDGE_CURVE('',#5162,#5175,#585,.F.);
#4186=EDGE_CURVE('',#5176,#5175,#586,.T.);
#4187=EDGE_CURVE('',#5163,#5176,#587,.T.);
#4188=EDGE_CURVE('',#5177,#5176,#588,.T.);
#4189=EDGE_CURVE('',#5164,#5177,#589,.F.);
#4190=EDGE_CURVE('',#5178,#5177,#590,.T.);
#4191=EDGE_CURVE('',#5165,#5178,#591,.T.);
#4192=EDGE_CURVE('',#5179,#5178,#5786,.F.);
#4193=EDGE_CURVE('',#5166,#5179,#592,.F.);
#4194=EDGE_CURVE('',#5180,#5179,#593,.T.);
#4195=EDGE_CURVE('',#5141,#5180,#594,.T.);
#4196=EDGE_CURVE('',#5181,#5180,#595,.T.);
#4197=EDGE_CURVE('',#5142,#5181,#5787,.T.);
#4198=EDGE_CURVE('',#5182,#5181,#596,.T.);
#4199=EDGE_CURVE('',#5143,#5182,#597,.F.);
#4200=EDGE_CURVE('',#5183,#5182,#598,.T.);
#4201=EDGE_CURVE('',#5144,#5183,#599,.T.);
#4202=EDGE_CURVE('',#5184,#5183,#5788,.F.);
#4203=EDGE_CURVE('',#5145,#5184,#600,.F.);
#4204=EDGE_CURVE('',#5185,#5184,#601,.T.);
#4205=EDGE_CURVE('',#5146,#5185,#602,.T.);
#4206=EDGE_CURVE('',#5186,#5185,#603,.T.);
#4207=EDGE_CURVE('',#5147,#5186,#604,.F.);
#4208=EDGE_CURVE('',#5187,#5186,#605,.T.);
#4209=EDGE_CURVE('',#5148,#5187,#606,.T.);
#4210=EDGE_CURVE('',#5188,#5187,#5789,.F.);
#4211=EDGE_CURVE('',#5149,#5188,#607,.F.);
#4212=EDGE_CURVE('',#5189,#5188,#608,.T.);
#4213=EDGE_CURVE('',#5150,#5189,#609,.T.);
#4214=EDGE_CURVE('',#5190,#5189,#610,.T.);
#4215=EDGE_CURVE('',#5151,#5190,#611,.F.);
#4216=EDGE_CURVE('',#5191,#5190,#612,.T.);
#4217=EDGE_CURVE('',#5152,#5191,#613,.T.);
#4218=EDGE_CURVE('',#5192,#5191,#5790,.F.);
#4219=EDGE_CURVE('',#5153,#5192,#614,.F.);
#4220=EDGE_CURVE('',#5169,#5192,#615,.T.);
#4221=EDGE_CURVE('',#5193,#5193,#5791,.T.);
#4222=EDGE_CURVE('',#5194,#5168,#616,.F.);
#4223=EDGE_CURVE('',#5169,#5195,#617,.F.);
#4224=EDGE_CURVE('',#5195,#5194,#5792,.F.);
#4225=EDGE_CURVE('',#5196,#5194,#5793,.F.);
#4226=EDGE_CURVE('',#5197,#5196,#618,.F.);
#4227=EDGE_CURVE('',#5170,#5197,#5794,.T.);
#4228=EDGE_CURVE('',#5198,#5198,#5795,.F.);
#4229=EDGE_CURVE('',#5199,#5200,#619,.T.);
#4230=EDGE_CURVE('',#5179,#5199,#5796,.F.);
#4231=EDGE_CURVE('',#5201,#5178,#5797,.F.);
#4232=EDGE_CURVE('',#5202,#5201,#620,.T.);
#4233=EDGE_CURVE('',#5203,#5202,#5798,.F.);
#4234=EDGE_CURVE('',#5204,#5203,#5799,.F.);
#4235=EDGE_CURVE('',#5205,#5204,#5800,.F.);
#4236=EDGE_CURVE('',#5206,#5205,#621,.T.);
#4237=EDGE_CURVE('',#5175,#5206,#5801,.F.);
#4238=EDGE_CURVE('',#5207,#5174,#5802,.F.);
#4239=EDGE_CURVE('',#5208,#5207,#622,.T.);
#4240=EDGE_CURVE('',#5209,#5208,#5803,.F.);
#4241=EDGE_CURVE('',#5210,#5209,#5804,.F.);
#4242=EDGE_CURVE('',#5211,#5210,#5805,.F.);
#4243=EDGE_CURVE('',#5212,#5211,#623,.T.);
#4244=EDGE_CURVE('',#5171,#5212,#5806,.F.);
#4245=EDGE_CURVE('',#5213,#5197,#624,.T.);
#4246=EDGE_CURVE('',#5214,#5213,#5807,.F.);
#4247=EDGE_CURVE('',#5215,#5214,#5808,.F.);
#4248=EDGE_CURVE('',#5216,#5215,#5809,.F.);
#4249=EDGE_CURVE('',#5217,#5216,#625,.T.);
#4250=EDGE_CURVE('',#5192,#5217,#5810,.F.);
#4251=EDGE_CURVE('',#5218,#5191,#5811,.F.);
#4252=EDGE_CURVE('',#5219,#5218,#626,.T.);
#4253=EDGE_CURVE('',#5220,#5219,#5812,.F.);
#4254=EDGE_CURVE('',#5221,#5220,#5813,.F.);
#4255=EDGE_CURVE('',#5222,#5221,#5814,.F.);
#4256=EDGE_CURVE('',#5223,#5222,#627,.T.);
#4257=EDGE_CURVE('',#5188,#5223,#5815,.F.);
#4258=EDGE_CURVE('',#5224,#5187,#5816,.F.);
#4259=EDGE_CURVE('',#5225,#5224,#628,.T.);
#4260=EDGE_CURVE('',#5226,#5225,#5817,.F.);
#4261=EDGE_CURVE('',#5227,#5226,#5818,.F.);
#4262=EDGE_CURVE('',#5228,#5227,#5819,.F.);
#4263=EDGE_CURVE('',#5229,#5228,#629,.T.);
#4264=EDGE_CURVE('',#5184,#5229,#5820,.F.);
#4265=EDGE_CURVE('',#5230,#5183,#5821,.F.);
#4266=EDGE_CURVE('',#5231,#5230,#630,.T.);
#4267=EDGE_CURVE('',#5232,#5231,#5822,.F.);
#4268=EDGE_CURVE('',#5233,#5232,#5823,.F.);
#4269=EDGE_CURVE('',#5200,#5233,#5824,.F.);
#4270=EDGE_CURVE('',#5234,#5234,#5825,.T.);
#4271=EDGE_CURVE('',#5235,#5235,#5826,.T.);
#4272=EDGE_CURVE('',#5236,#5236,#5827,.T.);
#4273=EDGE_CURVE('',#5237,#5237,#5828,.T.);
#4274=EDGE_CURVE('',#5238,#5238,#5829,.T.);
#4275=EDGE_CURVE('',#5239,#5239,#5830,.T.);
#4276=EDGE_CURVE('',#5240,#5240,#5831,.T.);
#4277=EDGE_CURVE('',#5241,#5241,#5832,.T.);
#4278=EDGE_CURVE('',#5242,#5242,#5833,.T.);
#4279=EDGE_CURVE('',#5243,#5243,#5834,.T.);
#4280=EDGE_CURVE('',#5244,#5244,#5835,.T.);
#4281=EDGE_CURVE('',#5245,#5245,#5836,.T.);
#4282=EDGE_CURVE('',#5246,#5246,#5837,.T.);
#4283=EDGE_CURVE('',#5247,#5247,#5838,.T.);
#4284=EDGE_CURVE('',#5248,#5248,#5839,.T.);
#4285=EDGE_CURVE('',#5249,#5249,#5840,.T.);
#4286=EDGE_CURVE('',#5250,#5250,#5841,.T.);
#4287=EDGE_CURVE('',#5251,#5251,#5842,.T.);
#4288=EDGE_CURVE('',#5252,#5212,#631,.F.);
#4289=EDGE_CURVE('',#5253,#5252,#5843,.F.);
#4290=EDGE_CURVE('',#5172,#5253,#632,.F.);
#4291=EDGE_CURVE('',#5254,#5173,#633,.F.);
#4292=EDGE_CURVE('',#5253,#5254,#5844,.F.);
#4293=EDGE_CURVE('',#5255,#5254,#5845,.F.);
#4294=EDGE_CURVE('',#5207,#5255,#634,.F.);
#4295=EDGE_CURVE('',#5256,#5206,#635,.F.);
#4296=EDGE_CURVE('',#5257,#5256,#5846,.F.);
#4297=EDGE_CURVE('',#5176,#5257,#636,.F.);
#4298=EDGE_CURVE('',#5257,#5258,#5847,.F.);
#4299=EDGE_CURVE('',#5258,#5177,#637,.F.);
#4300=EDGE_CURVE('',#5259,#5258,#5848,.F.);
#4301=EDGE_CURVE('',#5201,#5259,#638,.F.);
#4302=EDGE_CURVE('',#5260,#5199,#639,.F.);
#4303=EDGE_CURVE('',#5261,#5260,#5849,.F.);
#4304=EDGE_CURVE('',#5180,#5261,#640,.F.);
#4305=EDGE_CURVE('',#5261,#5262,#5850,.F.);
#4306=EDGE_CURVE('',#5262,#5182,#641,.F.);
#4307=EDGE_CURVE('',#5263,#5262,#5851,.F.);
#4308=EDGE_CURVE('',#5230,#5263,#642,.F.);
#4309=EDGE_CURVE('',#5264,#5229,#643,.F.);
#4310=EDGE_CURVE('',#5265,#5264,#5852,.F.);
#4311=EDGE_CURVE('',#5185,#5265,#644,.F.);
#4312=EDGE_CURVE('',#5265,#5266,#5853,.F.);
#4313=EDGE_CURVE('',#5266,#5186,#645,.F.);
#4314=EDGE_CURVE('',#5267,#5266,#5854,.F.);
#4315=EDGE_CURVE('',#5224,#5267,#646,.F.);
#4316=EDGE_CURVE('',#5268,#5223,#647,.F.);
#4317=EDGE_CURVE('',#5269,#5268,#5855,.F.);
#4318=EDGE_CURVE('',#5189,#5269,#648,.F.);
#4319=EDGE_CURVE('',#5270,#5190,#649,.F.);
#4320=EDGE_CURVE('',#5269,#5270,#5856,.F.);
#4321=EDGE_CURVE('',#5271,#5270,#5857,.F.);
#4322=EDGE_CURVE('',#5218,#5271,#650,.F.);
#4323=EDGE_CURVE('',#5195,#5272,#5858,.F.);
#4324=EDGE_CURVE('',#5272,#5217,#651,.F.);
#4325=EDGE_CURVE('',#5273,#5274,#5859,.F.);
#4326=EDGE_CURVE('',#5274,#5273,#652,.T.);
#4327=EDGE_CURVE('',#5275,#5275,#5860,.T.);
#4328=EDGE_CURVE('',#5276,#5276,#5861,.F.);
#4329=EDGE_CURVE('',#5277,#5278,#5862,.T.);
#4330=EDGE_CURVE('',#5255,#5277,#653,.T.);
#4331=EDGE_CURVE('',#5279,#5252,#654,.T.);
#4332=EDGE_CURVE('',#5280,#5279,#5863,.T.);
#4333=EDGE_CURVE('',#5278,#5280,#5864,.T.);
#4334=EDGE_CURVE('',#5281,#5256,#655,.T.);
#4335=EDGE_CURVE('',#5282,#5281,#5865,.T.);
#4336=EDGE_CURVE('',#5283,#5282,#5866,.T.);
#4337=EDGE_CURVE('',#5284,#5283,#5867,.T.);
#4338=EDGE_CURVE('',#5259,#5284,#656,.T.);
#4339=EDGE_CURVE('',#5285,#5260,#657,.T.);
#4340=EDGE_CURVE('',#5286,#5285,#5868,.T.);
#4341=EDGE_CURVE('',#5287,#5286,#5869,.T.);
#4342=EDGE_CURVE('',#5288,#5287,#5870,.T.);
#4343=EDGE_CURVE('',#5263,#5288,#658,.T.);
#4344=EDGE_CURVE('',#5289,#5264,#659,.T.);
#4345=EDGE_CURVE('',#5290,#5289,#5871,.T.);
#4346=EDGE_CURVE('',#5291,#5290,#5872,.T.);
#4347=EDGE_CURVE('',#5292,#5291,#5873,.T.);
#4348=EDGE_CURVE('',#5267,#5292,#660,.T.);
#4349=EDGE_CURVE('',#5293,#5268,#661,.T.);
#4350=EDGE_CURVE('',#5294,#5293,#5874,.T.);
#4351=EDGE_CURVE('',#5295,#5294,#5875,.T.);
#4352=EDGE_CURVE('',#5296,#5295,#5876,.T.);
#4353=EDGE_CURVE('',#5271,#5296,#662,.T.);
#4354=EDGE_CURVE('',#5297,#5298,#5877,.T.);
#4355=EDGE_CURVE('',#5196,#5297,#663,.T.);
#4356=EDGE_CURVE('',#5299,#5272,#664,.T.);
#4357=EDGE_CURVE('',#5300,#5299,#5878,.T.);
#4358=EDGE_CURVE('',#5298,#5300,#5879,.T.);
#4359=EDGE_CURVE('',#5301,#5301,#5880,.F.);
#4360=EDGE_CURVE('',#5302,#5302,#5881,.F.);
#4361=EDGE_CURVE('',#5303,#5303,#5882,.F.);
#4362=EDGE_CURVE('',#5304,#5304,#5883,.F.);
#4363=EDGE_CURVE('',#5305,#5305,#5884,.F.);
#4364=EDGE_CURVE('',#5306,#5306,#5885,.F.);
#4365=EDGE_CURVE('',#5307,#5307,#5886,.F.);
#4366=EDGE_CURVE('',#5308,#5308,#5887,.F.);
#4367=EDGE_CURVE('',#5309,#5309,#5888,.F.);
#4368=EDGE_CURVE('',#5310,#5310,#5889,.F.);
#4369=EDGE_CURVE('',#5311,#5311,#5890,.F.);
#4370=EDGE_CURVE('',#5312,#5312,#5891,.F.);
#4371=EDGE_CURVE('',#5313,#5313,#5892,.F.);
#4372=EDGE_CURVE('',#5314,#5314,#5893,.F.);
#4373=EDGE_CURVE('',#5315,#5315,#5894,.F.);
#4374=EDGE_CURVE('',#5316,#5316,#5895,.F.);
#4375=EDGE_CURVE('',#5317,#5317,#5896,.F.);
#4376=EDGE_CURVE('',#5318,#5318,#5897,.F.);
#4377=EDGE_CURVE('',#5213,#5297,#665,.T.);
#4378=EDGE_CURVE('',#5202,#5284,#666,.T.);
#4379=EDGE_CURVE('',#5203,#5283,#667,.F.);
#4380=EDGE_CURVE('',#5204,#5282,#668,.F.);
#4381=EDGE_CURVE('',#5205,#5281,#669,.F.);
#4382=EDGE_CURVE('',#5208,#5277,#670,.T.);
#4383=EDGE_CURVE('',#5209,#5278,#671,.F.);
#4384=EDGE_CURVE('',#5210,#5280,#672,.F.);
#4385=EDGE_CURVE('',#5211,#5279,#673,.F.);
#4386=EDGE_CURVE('',#5214,#5298,#674,.F.);
#4387=EDGE_CURVE('',#5215,#5300,#675,.F.);
#4388=EDGE_CURVE('',#5216,#5299,#676,.F.);
#4389=EDGE_CURVE('',#5219,#5296,#677,.T.);
#4390=EDGE_CURVE('',#5220,#5295,#678,.F.);
#4391=EDGE_CURVE('',#5221,#5294,#679,.F.);
#4392=EDGE_CURVE('',#5222,#5293,#680,.F.);
#4393=EDGE_CURVE('',#5225,#5292,#681,.T.);
#4394=EDGE_CURVE('',#5226,#5291,#682,.F.);
#4395=EDGE_CURVE('',#5227,#5290,#683,.F.);
#4396=EDGE_CURVE('',#5228,#5289,#684,.F.);
#4397=EDGE_CURVE('',#5231,#5288,#685,.T.);
#4398=EDGE_CURVE('',#5232,#5287,#686,.F.);
#4399=EDGE_CURVE('',#5233,#5286,#687,.F.);
#4400=EDGE_CURVE('',#5200,#5285,#688,.F.);
#4401=EDGE_CURVE('',#5319,#5320,#5898,.T.);
#4402=EDGE_CURVE('',#5320,#5319,#689,.T.);
#4403=EDGE_CURVE('',#5321,#5322,#5899,.T.);
#4404=EDGE_CURVE('',#5322,#5321,#690,.F.);
#4405=EDGE_CURVE('',#5323,#5324,#5900,.T.);
#4406=EDGE_CURVE('',#5324,#5323,#691,.T.);
#4407=EDGE_CURVE('',#5325,#5326,#5901,.F.);
#4408=EDGE_CURVE('',#5326,#5325,#692,.T.);
#4409=EDGE_CURVE('',#5327,#5327,#5902,.T.);
#4410=EDGE_CURVE('',#5328,#5329,#5903,.F.);
#4411=EDGE_CURVE('',#5329,#5328,#693,.F.);
#4412=EDGE_CURVE('',#5330,#5331,#5904,.F.);
#4413=EDGE_CURVE('',#5332,#5330,#694,.T.);
#4414=EDGE_CURVE('',#5333,#5332,#5905,.T.);
#4415=EDGE_CURVE('',#5334,#5333,#695,.T.);
#4416=EDGE_CURVE('',#5335,#5334,#5906,.F.);
#4417=EDGE_CURVE('',#5336,#5335,#696,.T.);
#4418=EDGE_CURVE('',#5337,#5336,#5907,.T.);
#4419=EDGE_CURVE('',#5338,#5337,#697,.T.);
#4420=EDGE_CURVE('',#5339,#5338,#5908,.F.);
#4421=EDGE_CURVE('',#5340,#5339,#698,.T.);
#4422=EDGE_CURVE('',#5341,#5340,#5909,.T.);
#4423=EDGE_CURVE('',#5342,#5341,#699,.T.);
#4424=EDGE_CURVE('',#5343,#5342,#5910,.F.);
#4425=EDGE_CURVE('',#5344,#5343,#700,.T.);
#4426=EDGE_CURVE('',#5345,#5344,#5911,.T.);
#4427=EDGE_CURVE('',#5346,#5345,#701,.T.);
#4428=EDGE_CURVE('',#5347,#5346,#5912,.F.);
#4429=EDGE_CURVE('',#5348,#5347,#702,.T.);
#4430=EDGE_CURVE('',#5349,#5348,#5913,.T.);
#4431=EDGE_CURVE('',#5350,#5349,#703,.T.);
#4432=EDGE_CURVE('',#5351,#5350,#5914,.F.);
#4433=EDGE_CURVE('',#5352,#5351,#704,.T.);
#4434=EDGE_CURVE('',#5353,#5352,#5915,.T.);
#4435=EDGE_CURVE('',#5331,#5353,#705,.T.);
#4436=EDGE_CURVE('',#5354,#5354,#5916,.F.);
#4437=EDGE_CURVE('',#5355,#5356,#5917,.F.);
#4438=EDGE_CURVE('',#5356,#5355,#5918,.F.);
#4439=EDGE_CURVE('',#5357,#5357,#5919,.F.);
#4440=EDGE_CURVE('',#5358,#5358,#5920,.F.);
#4441=EDGE_CURVE('',#5359,#5360,#5921,.F.);
#4442=EDGE_CURVE('',#5360,#5359,#5922,.F.);
#4443=EDGE_CURVE('',#5361,#5361,#5923,.F.);
#4444=EDGE_CURVE('',#5362,#5328,#5924,.F.);
#4445=EDGE_CURVE('',#5363,#5362,#706,.T.);
#4446=EDGE_CURVE('',#5364,#5363,#707,.T.);
#4447=EDGE_CURVE('',#5365,#5364,#708,.T.);
#4448=EDGE_CURVE('',#5366,#5365,#709,.T.);
#4449=EDGE_CURVE('',#5367,#5366,#710,.T.);
#4450=EDGE_CURVE('',#5368,#5367,#711,.T.);
#4451=EDGE_CURVE('',#5369,#5368,#5925,.T.);
#4452=EDGE_CURVE('',#5370,#5369,#712,.T.);
#4453=EDGE_CURVE('',#5371,#5370,#713,.T.);
#4454=EDGE_CURVE('',#5372,#5371,#714,.T.);
#4455=EDGE_CURVE('',#5373,#5372,#715,.T.);
#4456=EDGE_CURVE('',#5374,#5373,#716,.T.);
#4457=EDGE_CURVE('',#5375,#5374,#717,.T.);
#4458=EDGE_CURVE('',#5329,#5375,#5926,.T.);
#4459=EDGE_CURVE('',#5376,#5377,#718,.T.);
#4460=EDGE_CURVE('',#5362,#5376,#719,.T.);
#4461=EDGE_CURVE('',#5378,#5375,#720,.T.);
#4462=EDGE_CURVE('',#5379,#5378,#721,.T.);
#4463=EDGE_CURVE('',#5380,#5379,#722,.T.);
#4464=EDGE_CURVE('',#5381,#5380,#723,.T.);
#4465=EDGE_CURVE('',#5382,#5381,#724,.T.);
#4466=EDGE_CURVE('',#5383,#5382,#725,.T.);
#4467=EDGE_CURVE('',#5384,#5383,#726,.T.);
#4468=EDGE_CURVE('',#5385,#5384,#727,.T.);
#4469=EDGE_CURVE('',#5386,#5385,#728,.T.);
#4470=EDGE_CURVE('',#5387,#5386,#729,.T.);
#4471=EDGE_CURVE('',#5377,#5387,#730,.T.);
#4472=EDGE_CURVE('',#5388,#5389,#5927,.T.);
#4473=EDGE_CURVE('',#5389,#5388,#731,.T.);
#4474=EDGE_CURVE('',#5390,#5391,#5928,.T.);
#4475=EDGE_CURVE('',#5391,#5360,#732,.T.);
#4476=EDGE_CURVE('',#5359,#5390,#733,.T.);
#4477=EDGE_CURVE('',#5391,#5390,#734,.T.);
#4478=EDGE_CURVE('',#5392,#5393,#735,.T.);
#4479=EDGE_CURVE('',#5393,#5394,#5929,.F.);
#4480=EDGE_CURVE('',#5394,#5392,#5930,.T.);
#4481=EDGE_CURVE('',#5395,#5396,#736,.T.);
#4482=EDGE_CURVE('',#5396,#5397,#5931,.F.);
#4483=EDGE_CURVE('',#5397,#5395,#5932,.T.);
#4484=EDGE_CURVE('',#5398,#5399,#5933,.T.);
#4485=EDGE_CURVE('',#5399,#5356,#737,.T.);
#4486=EDGE_CURVE('',#5355,#5398,#738,.T.);
#4487=EDGE_CURVE('',#5399,#5398,#5934,.T.);
#4488=EDGE_CURVE('',#5400,#5401,#739,.T.);
#4489=EDGE_CURVE('',#5401,#5400,#5935,.T.);
#4490=EDGE_CURVE('',#5402,#5380,#740,.T.);
#4491=EDGE_CURVE('',#5403,#5402,#741,.T.);
#4492=EDGE_CURVE('',#5332,#5403,#742,.T.);
#4493=EDGE_CURVE('',#5381,#5330,#743,.T.);
#4494=EDGE_CURVE('',#5403,#5404,#744,.T.);
#4495=EDGE_CURVE('',#5404,#5405,#745,.T.);
#4496=EDGE_CURVE('',#5405,#5406,#746,.T.);
#4497=EDGE_CURVE('',#5406,#5333,#747,.T.);
#4498=EDGE_CURVE('',#5407,#5406,#748,.T.);
#4499=EDGE_CURVE('',#5379,#5407,#749,.T.);
#4500=EDGE_CURVE('',#5334,#5378,#750,.T.);
#4501=EDGE_CURVE('',#5374,#5335,#751,.F.);
#4502=EDGE_CURVE('',#5408,#5373,#752,.T.);
#4503=EDGE_CURVE('',#5409,#5408,#753,.T.);
#4504=EDGE_CURVE('',#5336,#5409,#754,.T.);
#4505=EDGE_CURVE('',#5409,#5410,#755,.T.);
#4506=EDGE_CURVE('',#5410,#5411,#756,.T.);
#4507=EDGE_CURVE('',#5411,#5412,#757,.F.);
#4508=EDGE_CURVE('',#5412,#5337,#758,.T.);
#4509=EDGE_CURVE('',#5413,#5412,#759,.T.);
#4510=EDGE_CURVE('',#5372,#5413,#760,.T.);
#4511=EDGE_CURVE('',#5338,#5371,#761,.T.);
#4512=EDGE_CURVE('',#5370,#5414,#762,.F.);
#4513=EDGE_CURVE('',#5414,#5339,#763,.T.);
#4514=EDGE_CURVE('',#5414,#5415,#764,.F.);
#4515=EDGE_CURVE('',#5415,#5340,#5936,.F.);
#4516=EDGE_CURVE('',#5340,#5416,#5937,.T.);
#4517=EDGE_CURVE('',#5416,#5417,#5938,.F.);
#4518=EDGE_CURVE('',#5417,#5418,#765,.F.);
#4519=EDGE_CURVE('',#5418,#5341,#766,.T.);
#4520=EDGE_CURVE('',#5342,#5367,#767,.T.);
#4521=EDGE_CURVE('',#5419,#5418,#768,.T.);
#4522=EDGE_CURVE('',#5368,#5419,#769,.T.);
#4523=EDGE_CURVE('',#5366,#5343,#770,.F.);
#4524=EDGE_CURVE('',#5420,#5365,#771,.T.);
#4525=EDGE_CURVE('',#5421,#5420,#772,.T.);
#4526=EDGE_CURVE('',#5344,#5421,#773,.T.);
#4527=EDGE_CURVE('',#5421,#5422,#774,.T.);
#4528=EDGE_CURVE('',#5422,#5423,#775,.T.);
#4529=EDGE_CURVE('',#5423,#5424,#776,.F.);
#4530=EDGE_CURVE('',#5424,#5345,#777,.T.);
#4531=EDGE_CURVE('',#5425,#5424,#778,.T.);
#4532=EDGE_CURVE('',#5364,#5425,#779,.T.);
#4533=EDGE_CURVE('',#5346,#5363,#780,.T.);
#4534=EDGE_CURVE('',#5376,#5347,#781,.F.);
#4535=EDGE_CURVE('',#5426,#5377,#782,.T.);
#4536=EDGE_CURVE('',#5427,#5426,#783,.T.);
#4537=EDGE_CURVE('',#5348,#5427,#784,.T.);
#4538=EDGE_CURVE('',#5427,#5428,#785,.T.);
#4539=EDGE_CURVE('',#5428,#5429,#786,.T.);
#4540=EDGE_CURVE('',#5429,#5430,#787,.F.);
#4541=EDGE_CURVE('',#5430,#5349,#788,.T.);
#4542=EDGE_CURVE('',#5431,#5430,#789,.T.);
#4543=EDGE_CURVE('',#5387,#5431,#790,.T.);
#4544=EDGE_CURVE('',#5350,#5386,#791,.T.);
#4545=EDGE_CURVE('',#5385,#5351,#792,.F.);
#4546=EDGE_CURVE('',#5432,#5384,#793,.T.);
#4547=EDGE_CURVE('',#5433,#5432,#794,.T.);
#4548=EDGE_CURVE('',#5352,#5433,#795,.T.);
#4549=EDGE_CURVE('',#5433,#5434,#796,.T.);
#4550=EDGE_CURVE('',#5434,#5435,#797,.T.);
#4551=EDGE_CURVE('',#5435,#5436,#798,.F.);
#4552=EDGE_CURVE('',#5436,#5353,#799,.T.);
#4553=EDGE_CURVE('',#5437,#5436,#800,.T.);
#4554=EDGE_CURVE('',#5383,#5437,#801,.T.);
#4555=EDGE_CURVE('',#5331,#5382,#802,.T.);
#4556=EDGE_CURVE('',#5425,#5438,#803,.T.);
#4557=EDGE_CURVE('',#5438,#5439,#804,.F.);
#4558=EDGE_CURVE('',#5439,#5420,#805,.T.);
#4559=EDGE_CURVE('',#5440,#5441,#806,.F.);
#4560=EDGE_CURVE('',#5441,#5440,#807,.F.);
#4561=EDGE_CURVE('',#5419,#5442,#808,.T.);
#4562=EDGE_CURVE('',#5442,#5443,#5939,.F.);
#4563=EDGE_CURVE('',#5444,#5443,#809,.F.);
#4564=EDGE_CURVE('',#5444,#5369,#810,.T.);
#4565=EDGE_CURVE('',#5445,#5446,#811,.F.);
#4566=EDGE_CURVE('',#5446,#5445,#812,.F.);
#4567=EDGE_CURVE('',#5415,#5444,#813,.T.);
#4568=EDGE_CURVE('',#5413,#5447,#814,.T.);
#4569=EDGE_CURVE('',#5447,#5448,#815,.F.);
#4570=EDGE_CURVE('',#5448,#5408,#816,.T.);
#4571=EDGE_CURVE('',#5449,#5450,#817,.F.);
#4572=EDGE_CURVE('',#5450,#5449,#818,.F.);
#4573=EDGE_CURVE('',#5407,#5451,#819,.T.);
#4574=EDGE_CURVE('',#5451,#5452,#820,.F.);
#4575=EDGE_CURVE('',#5452,#5402,#821,.T.);
#4576=EDGE_CURVE('',#5453,#5454,#822,.F.);
#4577=EDGE_CURVE('',#5454,#5453,#823,.F.);
#4578=EDGE_CURVE('',#5437,#5455,#824,.T.);
#4579=EDGE_CURVE('',#5455,#5456,#825,.F.);
#4580=EDGE_CURVE('',#5456,#5432,#826,.T.);
#4581=EDGE_CURVE('',#5457,#5458,#827,.F.);
#4582=EDGE_CURVE('',#5458,#5457,#828,.F.);
#4583=EDGE_CURVE('',#5431,#5459,#829,.T.);
#4584=EDGE_CURVE('',#5459,#5460,#830,.F.);
#4585=EDGE_CURVE('',#5460,#5426,#831,.T.);
#4586=EDGE_CURVE('',#5461,#5462,#832,.F.);
#4587=EDGE_CURVE('',#5462,#5461,#833,.F.);
#4588=EDGE_CURVE('',#5463,#5464,#834,.F.);
#4589=EDGE_CURVE('',#5465,#5463,#835,.F.);
#4590=EDGE_CURVE('',#5466,#5465,#836,.F.);
#4591=EDGE_CURVE('',#5464,#5466,#837,.F.);
#4592=EDGE_CURVE('',#5467,#5468,#838,.F.);
#4593=EDGE_CURVE('',#5469,#5467,#839,.F.);
#4594=EDGE_CURVE('',#5470,#5469,#840,.F.);
#4595=EDGE_CURVE('',#5468,#5470,#841,.F.);
#4596=EDGE_CURVE('',#5471,#5472,#842,.F.);
#4597=EDGE_CURVE('',#5473,#5471,#843,.F.);
#4598=EDGE_CURVE('',#5474,#5473,#844,.F.);
#4599=EDGE_CURVE('',#5472,#5474,#845,.F.);
#4600=EDGE_CURVE('',#5475,#5476,#846,.F.);
#4601=EDGE_CURVE('',#5477,#5475,#847,.F.);
#4602=EDGE_CURVE('',#5478,#5477,#848,.F.);
#4603=EDGE_CURVE('',#5476,#5478,#849,.F.);
#4604=EDGE_CURVE('',#5479,#5480,#850,.F.);
#4605=EDGE_CURVE('',#5481,#5479,#851,.F.);
#4606=EDGE_CURVE('',#5482,#5481,#852,.F.);
#4607=EDGE_CURVE('',#5480,#5482,#853,.F.);
#4608=EDGE_CURVE('',#5483,#5484,#854,.F.);
#4609=EDGE_CURVE('',#5485,#5483,#855,.F.);
#4610=EDGE_CURVE('',#5486,#5485,#856,.F.);
#4611=EDGE_CURVE('',#5484,#5486,#857,.F.);
#4612=EDGE_CURVE('',#5452,#5487,#858,.T.);
#4613=EDGE_CURVE('',#5487,#5404,#859,.F.);
#4614=EDGE_CURVE('',#5488,#5405,#860,.F.);
#4615=EDGE_CURVE('',#5488,#5451,#861,.T.);
#4616=EDGE_CURVE('',#5487,#5488,#862,.F.);
#4617=EDGE_CURVE('',#5448,#5489,#863,.T.);
#4618=EDGE_CURVE('',#5410,#5489,#864,.F.);
#4619=EDGE_CURVE('',#5490,#5447,#865,.F.);
#4620=EDGE_CURVE('',#5411,#5490,#866,.F.);
#4621=EDGE_CURVE('',#5489,#5490,#867,.F.);
#4622=EDGE_CURVE('',#5415,#5416,#868,.F.);
#4623=EDGE_CURVE('',#5417,#5491,#869,.F.);
#4624=EDGE_CURVE('',#5491,#5442,#870,.F.);
#4625=EDGE_CURVE('',#5416,#5492,#871,.F.);
#4626=EDGE_CURVE('',#5492,#5491,#5940,.T.);
#4627=EDGE_CURVE('',#5439,#5493,#872,.T.);
#4628=EDGE_CURVE('',#5493,#5422,#873,.F.);
#4629=EDGE_CURVE('',#5494,#5438,#874,.F.);
#4630=EDGE_CURVE('',#5423,#5494,#875,.F.);
#4631=EDGE_CURVE('',#5493,#5494,#876,.F.);
#4632=EDGE_CURVE('',#5460,#5495,#877,.T.);
#4633=EDGE_CURVE('',#5495,#5428,#878,.F.);
#4634=EDGE_CURVE('',#5496,#5459,#879,.F.);
#4635=EDGE_CURVE('',#5429,#5496,#880,.F.);
#4636=EDGE_CURVE('',#5495,#5496,#881,.F.);
#4637=EDGE_CURVE('',#5456,#5497,#882,.T.);
#4638=EDGE_CURVE('',#5497,#5434,#883,.F.);
#4639=EDGE_CURVE('',#5498,#5455,#884,.F.);
#4640=EDGE_CURVE('',#5435,#5498,#885,.F.);
#4641=EDGE_CURVE('',#5497,#5498,#886,.F.);
#4642=EDGE_CURVE('',#5464,#5440,#5941,.T.);
#4643=EDGE_CURVE('',#5441,#5465,#5942,.T.);
#4644=EDGE_CURVE('',#5468,#5445,#5943,.T.);
#4645=EDGE_CURVE('',#5446,#5469,#5944,.T.);
#4646=EDGE_CURVE('',#5492,#5443,#887,.F.);
#4647=EDGE_CURVE('',#5474,#5449,#5945,.T.);
#4648=EDGE_CURVE('',#5450,#5471,#5946,.T.);
#4649=EDGE_CURVE('',#5478,#5453,#5947,.T.);
#4650=EDGE_CURVE('',#5454,#5475,#5948,.T.);
#4651=EDGE_CURVE('',#5482,#5457,#5949,.T.);
#4652=EDGE_CURVE('',#5458,#5479,#5950,.T.);
#4653=EDGE_CURVE('',#5484,#5461,#5951,.T.);
#4654=EDGE_CURVE('',#5462,#5485,#5952,.T.);
#4655=VERTEX_POINT('',#11101);
#4656=VERTEX_POINT('',#11103);
#4657=VERTEX_POINT('',#11106);
#4658=VERTEX_POINT('',#11109);
#4659=VERTEX_POINT('',#11112);
#4660=VERTEX_POINT('',#11113);
#4661=VERTEX_POINT('',#11118);
#4662=VERTEX_POINT('',#11120);
#4663=VERTEX_POINT('',#11125);
#4664=VERTEX_POINT('',#11127);
#4665=VERTEX_POINT('',#11132);
#4666=VERTEX_POINT('',#11134);
#4667=VERTEX_POINT('',#11139);
#4668=VERTEX_POINT('',#11141);
#4669=VERTEX_POINT('',#11146);
#4670=VERTEX_POINT('',#11148);
#4671=VERTEX_POINT('',#11153);
#4672=VERTEX_POINT('',#11155);
#4673=VERTEX_POINT('',#11160);
#4674=VERTEX_POINT('',#11162);
#4675=VERTEX_POINT('',#11167);
#4676=VERTEX_POINT('',#11169);
#4677=VERTEX_POINT('',#11174);
#4678=VERTEX_POINT('',#11176);
#4679=VERTEX_POINT('',#11181);
#4680=VERTEX_POINT('',#11183);
#4681=VERTEX_POINT('',#11188);
#4682=VERTEX_POINT('',#11190);
#4683=VERTEX_POINT('',#11195);
#4684=VERTEX_POINT('',#11197);
#4685=VERTEX_POINT('',#11202);
#4686=VERTEX_POINT('',#11204);
#4687=VERTEX_POINT('',#11209);
#4688=VERTEX_POINT('',#11211);
#4689=VERTEX_POINT('',#11216);
#4690=VERTEX_POINT('',#11218);
#4691=VERTEX_POINT('',#11223);
#4692=VERTEX_POINT('',#11225);
#4693=VERTEX_POINT('',#11230);
#4694=VERTEX_POINT('',#11232);
#4695=VERTEX_POINT('',#11237);
#4696=VERTEX_POINT('',#11239);
#4697=VERTEX_POINT('',#11244);
#4698=VERTEX_POINT('',#11246);
#4699=VERTEX_POINT('',#11251);
#4700=VERTEX_POINT('',#11253);
#4701=VERTEX_POINT('',#11258);
#4702=VERTEX_POINT('',#11260);
#4703=VERTEX_POINT('',#11265);
#4704=VERTEX_POINT('',#11267);
#4705=VERTEX_POINT('',#11272);
#4706=VERTEX_POINT('',#11274);
#4707=VERTEX_POINT('',#11279);
#4708=VERTEX_POINT('',#11281);
#4709=VERTEX_POINT('',#11286);
#4710=VERTEX_POINT('',#11288);
#4711=VERTEX_POINT('',#11293);
#4712=VERTEX_POINT('',#11295);
#4713=VERTEX_POINT('',#11300);
#4714=VERTEX_POINT('',#11302);
#4715=VERTEX_POINT('',#11307);
#4716=VERTEX_POINT('',#11309);
#4717=VERTEX_POINT('',#11314);
#4718=VERTEX_POINT('',#11316);
#4719=VERTEX_POINT('',#11321);
#4720=VERTEX_POINT('',#11323);
#4721=VERTEX_POINT('',#11328);
#4722=VERTEX_POINT('',#11330);
#4723=VERTEX_POINT('',#11335);
#4724=VERTEX_POINT('',#11337);
#4725=VERTEX_POINT('',#11342);
#4726=VERTEX_POINT('',#11344);
#4727=VERTEX_POINT('',#11349);
#4728=VERTEX_POINT('',#11351);
#4729=VERTEX_POINT('',#11356);
#4730=VERTEX_POINT('',#11358);
#4731=VERTEX_POINT('',#11363);
#4732=VERTEX_POINT('',#11365);
#4733=VERTEX_POINT('',#11370);
#4734=VERTEX_POINT('',#11372);
#4735=VERTEX_POINT('',#11377);
#4736=VERTEX_POINT('',#11379);
#4737=VERTEX_POINT('',#11384);
#4738=VERTEX_POINT('',#11386);
#4739=VERTEX_POINT('',#11393);
#4740=VERTEX_POINT('',#11399);
#4741=VERTEX_POINT('',#11401);
#4742=VERTEX_POINT('',#11411);
#4743=VERTEX_POINT('',#11416);
#4744=VERTEX_POINT('',#11423);
#4745=VERTEX_POINT('',#11424);
#4746=VERTEX_POINT('',#11429);
#4747=VERTEX_POINT('',#11443);
#4748=VERTEX_POINT('',#11448);
#4749=VERTEX_POINT('',#11455);
#4750=VERTEX_POINT('',#11465);
#4751=VERTEX_POINT('',#11470);
#4752=VERTEX_POINT('',#11480);
#4753=VERTEX_POINT('',#11482);
#4754=VERTEX_POINT('',#11487);
#4755=VERTEX_POINT('',#11497);
#4756=VERTEX_POINT('',#11502);
#4757=VERTEX_POINT('',#11509);
#4758=VERTEX_POINT('',#11519);
#4759=VERTEX_POINT('',#11524);
#4760=VERTEX_POINT('',#11534);
#4761=VERTEX_POINT('',#11536);
#4762=VERTEX_POINT('',#11541);
#4763=VERTEX_POINT('',#11551);
#4764=VERTEX_POINT('',#11556);
#4765=VERTEX_POINT('',#11563);
#4766=VERTEX_POINT('',#11573);
#4767=VERTEX_POINT('',#11578);
#4768=VERTEX_POINT('',#11588);
#4769=VERTEX_POINT('',#11590);
#4770=VERTEX_POINT('',#11595);
#4771=VERTEX_POINT('',#11605);
#4772=VERTEX_POINT('',#11610);
#4773=VERTEX_POINT('',#11617);
#4774=VERTEX_POINT('',#11627);
#4775=VERTEX_POINT('',#11632);
#4776=VERTEX_POINT('',#11642);
#4777=VERTEX_POINT('',#11644);
#4778=VERTEX_POINT('',#11649);
#4779=VERTEX_POINT('',#11659);
#4780=VERTEX_POINT('',#11664);
#4781=VERTEX_POINT('',#11671);
#4782=VERTEX_POINT('',#11681);
#4783=VERTEX_POINT('',#11686);
#4784=VERTEX_POINT('',#11696);
#4785=VERTEX_POINT('',#11698);
#4786=VERTEX_POINT('',#11703);
#4787=VERTEX_POINT('',#11713);
#4788=VERTEX_POINT('',#11718);
#4789=VERTEX_POINT('',#11725);
#4790=VERTEX_POINT('',#11735);
#4791=VERTEX_POINT('',#11740);
#4792=VERTEX_POINT('',#11750);
#4793=VERTEX_POINT('',#11752);
#4794=VERTEX_POINT('',#11757);
#4795=VERTEX_POINT('',#11767);
#4796=VERTEX_POINT('',#11772);
#4797=VERTEX_POINT('',#11779);
#4798=VERTEX_POINT('',#11789);
#4799=VERTEX_POINT('',#11794);
#4800=VERTEX_POINT('',#11804);
#4801=VERTEX_POINT('',#11806);
#4802=VERTEX_POINT('',#11811);
#4803=VERTEX_POINT('',#11821);
#4804=VERTEX_POINT('',#11826);
#4805=VERTEX_POINT('',#11833);
#4806=VERTEX_POINT('',#11843);
#4807=VERTEX_POINT('',#11848);
#4808=VERTEX_POINT('',#11858);
#4809=VERTEX_POINT('',#11860);
#4810=VERTEX_POINT('',#11865);
#4811=VERTEX_POINT('',#11875);
#4812=VERTEX_POINT('',#11880);
#4813=VERTEX_POINT('',#11887);
#4814=VERTEX_POINT('',#11897);
#4815=VERTEX_POINT('',#11902);
#4816=VERTEX_POINT('',#11912);
#4817=VERTEX_POINT('',#11914);
#4818=VERTEX_POINT('',#11919);
#4819=VERTEX_POINT('',#11929);
#4820=VERTEX_POINT('',#11934);
#4821=VERTEX_POINT('',#11941);
#4822=VERTEX_POINT('',#11951);
#4823=VERTEX_POINT('',#11956);
#4824=VERTEX_POINT('',#11966);
#4825=VERTEX_POINT('',#11968);
#4826=VERTEX_POINT('',#11973);
#4827=VERTEX_POINT('',#11983);
#4828=VERTEX_POINT('',#11988);
#4829=VERTEX_POINT('',#11995);
#4830=VERTEX_POINT('',#12005);
#4831=VERTEX_POINT('',#12010);
#4832=VERTEX_POINT('',#12020);
#4833=VERTEX_POINT('',#12022);
#4834=VERTEX_POINT('',#12027);
#4835=VERTEX_POINT('',#12037);
#4836=VERTEX_POINT('',#12042);
#4837=VERTEX_POINT('',#12049);
#4838=VERTEX_POINT('',#12059);
#4839=VERTEX_POINT('',#12064);
#4840=VERTEX_POINT('',#12074);
#4841=VERTEX_POINT('',#12076);
#4842=VERTEX_POINT('',#12081);
#4843=VERTEX_POINT('',#12091);
#4844=VERTEX_POINT('',#12096);
#4845=VERTEX_POINT('',#12103);
#4846=VERTEX_POINT('',#12113);
#4847=VERTEX_POINT('',#12118);
#4848=VERTEX_POINT('',#12128);
#4849=VERTEX_POINT('',#12130);
#4850=VERTEX_POINT('',#12135);
#4851=VERTEX_POINT('',#12145);
#4852=VERTEX_POINT('',#12150);
#4853=VERTEX_POINT('',#12157);
#4854=VERTEX_POINT('',#12167);
#4855=VERTEX_POINT('',#12172);
#4856=VERTEX_POINT('',#12182);
#4857=VERTEX_POINT('',#12184);
#4858=VERTEX_POINT('',#12189);
#4859=VERTEX_POINT('',#12199);
#4860=VERTEX_POINT('',#12204);
#4861=VERTEX_POINT('',#12211);
#4862=VERTEX_POINT('',#12221);
#4863=VERTEX_POINT('',#12226);
#4864=VERTEX_POINT('',#12236);
#4865=VERTEX_POINT('',#12238);
#4866=VERTEX_POINT('',#12243);
#4867=VERTEX_POINT('',#12253);
#4868=VERTEX_POINT('',#12258);
#4869=VERTEX_POINT('',#12265);
#4870=VERTEX_POINT('',#12275);
#4871=VERTEX_POINT('',#12280);
#4872=VERTEX_POINT('',#12290);
#4873=VERTEX_POINT('',#12292);
#4874=VERTEX_POINT('',#12297);
#4875=VERTEX_POINT('',#12307);
#4876=VERTEX_POINT('',#12312);
#4877=VERTEX_POINT('',#12319);
#4878=VERTEX_POINT('',#12329);
#4879=VERTEX_POINT('',#12334);
#4880=VERTEX_POINT('',#12344);
#4881=VERTEX_POINT('',#12346);
#4882=VERTEX_POINT('',#12351);
#4883=VERTEX_POINT('',#12361);
#4884=VERTEX_POINT('',#12366);
#4885=VERTEX_POINT('',#12373);
#4886=VERTEX_POINT('',#12383);
#4887=VERTEX_POINT('',#12388);
#4888=VERTEX_POINT('',#12398);
#4889=VERTEX_POINT('',#12400);
#4890=VERTEX_POINT('',#12405);
#4891=VERTEX_POINT('',#12415);
#4892=VERTEX_POINT('',#12420);
#4893=VERTEX_POINT('',#12427);
#4894=VERTEX_POINT('',#12437);
#4895=VERTEX_POINT('',#12442);
#4896=VERTEX_POINT('',#12452);
#4897=VERTEX_POINT('',#12454);
#4898=VERTEX_POINT('',#12459);
#4899=VERTEX_POINT('',#12469);
#4900=VERTEX_POINT('',#12476);
#4901=VERTEX_POINT('',#12484);
#4902=VERTEX_POINT('',#12494);
#4903=VERTEX_POINT('',#12504);
#4904=VERTEX_POINT('',#12506);
#4905=VERTEX_POINT('',#12515);
#4906=VERTEX_POINT('',#12517);
#4907=VERTEX_POINT('',#12526);
#4908=VERTEX_POINT('',#12528);
#4909=VERTEX_POINT('',#12537);
#4910=VERTEX_POINT('',#12539);
#4911=VERTEX_POINT('',#12548);
#4912=VERTEX_POINT('',#12550);
#4913=VERTEX_POINT('',#12559);
#4914=VERTEX_POINT('',#12561);
#4915=VERTEX_POINT('',#12570);
#4916=VERTEX_POINT('',#12572);
#4917=VERTEX_POINT('',#12581);
#4918=VERTEX_POINT('',#12583);
#4919=VERTEX_POINT('',#12592);
#4920=VERTEX_POINT('',#12594);
#4921=VERTEX_POINT('',#12603);
#4922=VERTEX_POINT('',#12606);
#4923=VERTEX_POINT('',#12615);
#4924=VERTEX_POINT('',#12617);
#4925=VERTEX_POINT('',#12626);
#4926=VERTEX_POINT('',#12628);
#4927=VERTEX_POINT('',#12637);
#4928=VERTEX_POINT('',#12639);
#4929=VERTEX_POINT('',#12648);
#4930=VERTEX_POINT('',#12650);
#4931=VERTEX_POINT('',#12659);
#4932=VERTEX_POINT('',#12661);
#4933=VERTEX_POINT('',#12670);
#4934=VERTEX_POINT('',#12672);
#4935=VERTEX_POINT('',#12681);
#4936=VERTEX_POINT('',#12683);
#4937=VERTEX_POINT('',#12692);
#4938=VERTEX_POINT('',#12694);
#4939=VERTEX_POINT('',#12703);
#4940=VERTEX_POINT('',#12705);
#4941=VERTEX_POINT('',#12711);
#4942=VERTEX_POINT('',#12942);
#4943=VERTEX_POINT('',#12947);
#4944=VERTEX_POINT('',#12968);
#4945=VERTEX_POINT('',#12973);
#4946=VERTEX_POINT('',#12975);
#4947=VERTEX_POINT('',#12978);
#4948=VERTEX_POINT('',#12981);
#4949=VERTEX_POINT('',#12984);
#4950=VERTEX_POINT('',#12985);
#4951=VERTEX_POINT('',#12999);
#4952=VERTEX_POINT('',#13012);
#4953=VERTEX_POINT('',#13013);
#4954=VERTEX_POINT('',#13023);
#4955=VERTEX_POINT('',#13024);
#4956=VERTEX_POINT('',#13028);
#4957=VERTEX_POINT('',#13037);
#4958=VERTEX_POINT('',#13038);
#4959=VERTEX_POINT('',#13042);
#4960=VERTEX_POINT('',#13043);
#4961=VERTEX_POINT('',#13060);
#4962=VERTEX_POINT('',#13068);
#4963=VERTEX_POINT('',#13087);
#4964=VERTEX_POINT('',#13088);
#4965=VERTEX_POINT('',#13092);
#4966=VERTEX_POINT('',#13093);
#4967=VERTEX_POINT('',#13110);
#4968=VERTEX_POINT('',#13112);
#4969=VERTEX_POINT('',#13134);
#4970=VERTEX_POINT('',#13146);
#4971=VERTEX_POINT('',#13157);
#4972=VERTEX_POINT('',#13159);
#4973=VERTEX_POINT('',#13162);
#4974=VERTEX_POINT('',#13165);
#4975=VERTEX_POINT('',#13168);
#4976=VERTEX_POINT('',#13169);
#4977=VERTEX_POINT('',#13183);
#4978=VERTEX_POINT('',#13196);
#4979=VERTEX_POINT('',#13197);
#4980=VERTEX_POINT('',#13207);
#4981=VERTEX_POINT('',#13208);
#4982=VERTEX_POINT('',#13212);
#4983=VERTEX_POINT('',#13221);
#4984=VERTEX_POINT('',#13222);
#4985=VERTEX_POINT('',#13226);
#4986=VERTEX_POINT('',#13227);
#4987=VERTEX_POINT('',#13244);
#4988=VERTEX_POINT('',#13252);
#4989=VERTEX_POINT('',#13271);
#4990=VERTEX_POINT('',#13272);
#4991=VERTEX_POINT('',#13276);
#4992=VERTEX_POINT('',#13277);
#4993=VERTEX_POINT('',#13294);
#4994=VERTEX_POINT('',#13296);
#4995=VERTEX_POINT('',#13318);
#4996=VERTEX_POINT('',#13330);
#4997=VERTEX_POINT('',#13351);
#4998=VERTEX_POINT('',#13352);
#4999=VERTEX_POINT('',#13355);
#5000=VERTEX_POINT('',#13358);
#5001=VERTEX_POINT('',#13371);
#5002=VERTEX_POINT('',#13372);
#5003=VERTEX_POINT('',#13386);
#5004=VERTEX_POINT('',#13387);
#5005=VERTEX_POINT('',#13391);
#5006=VERTEX_POINT('',#13398);
#5007=VERTEX_POINT('',#13410);
#5008=VERTEX_POINT('',#13420);
#5009=VERTEX_POINT('',#13423);
#5010=VERTEX_POINT('',#13436);
#5011=VERTEX_POINT('',#13437);
#5012=VERTEX_POINT('',#13441);
#5013=VERTEX_POINT('',#13442);
#5014=VERTEX_POINT('',#13450);
#5015=VERTEX_POINT('',#13456);
#5016=VERTEX_POINT('',#13475);
#5017=VERTEX_POINT('',#13480);
#5018=VERTEX_POINT('',#13492);
#5019=VERTEX_POINT('',#13501);
#5020=VERTEX_POINT('',#13502);
#5021=VERTEX_POINT('',#13506);
#5022=VERTEX_POINT('',#13507);
#5023=VERTEX_POINT('',#13532);
#5024=VERTEX_POINT('',#13533);
#5025=VERTEX_POINT('',#13536);
#5026=VERTEX_POINT('',#13539);
#5027=VERTEX_POINT('',#13552);
#5028=VERTEX_POINT('',#13553);
#5029=VERTEX_POINT('',#13567);
#5030=VERTEX_POINT('',#13568);
#5031=VERTEX_POINT('',#13572);
#5032=VERTEX_POINT('',#13579);
#5033=VERTEX_POINT('',#13591);
#5034=VERTEX_POINT('',#13601);
#5035=VERTEX_POINT('',#13604);
#5036=VERTEX_POINT('',#13617);
#5037=VERTEX_POINT('',#13618);
#5038=VERTEX_POINT('',#13622);
#5039=VERTEX_POINT('',#13623);
#5040=VERTEX_POINT('',#13631);
#5041=VERTEX_POINT('',#13637);
#5042=VERTEX_POINT('',#13656);
#5043=VERTEX_POINT('',#13661);
#5044=VERTEX_POINT('',#13673);
#5045=VERTEX_POINT('',#13682);
#5046=VERTEX_POINT('',#13683);
#5047=VERTEX_POINT('',#13687);
#5048=VERTEX_POINT('',#13688);
#5049=VERTEX_POINT('',#13703);
#5050=VERTEX_POINT('',#13705);
#5051=VERTEX_POINT('',#13708);
#5052=VERTEX_POINT('',#13711);
#5053=VERTEX_POINT('',#13714);
#5054=VERTEX_POINT('',#13717);
#5055=VERTEX_POINT('',#13720);
#5056=VERTEX_POINT('',#13723);
#5057=VERTEX_POINT('',#13726);
#5058=VERTEX_POINT('',#13729);
#5059=VERTEX_POINT('',#13732);
#5060=VERTEX_POINT('',#13735);
#5061=VERTEX_POINT('',#13738);
#5062=VERTEX_POINT('',#13741);
#5063=VERTEX_POINT('',#13744);
#5064=VERTEX_POINT('',#13747);
#5065=VERTEX_POINT('',#13750);
#5066=VERTEX_POINT('',#13753);
#5067=VERTEX_POINT('',#13756);
#5068=VERTEX_POINT('',#13759);
#5069=VERTEX_POINT('',#13762);
#5070=VERTEX_POINT('',#13765);
#5071=VERTEX_POINT('',#13768);
#5072=VERTEX_POINT('',#13771);
#5073=VERTEX_POINT('',#13774);
#5074=VERTEX_POINT('',#13777);
#5075=VERTEX_POINT('',#13780);
#5076=VERTEX_POINT('',#13783);
#5077=VERTEX_POINT('',#13786);
#5078=VERTEX_POINT('',#13789);
#5079=VERTEX_POINT('',#13792);
#5080=VERTEX_POINT('',#13795);
#5081=VERTEX_POINT('',#13798);
#5082=VERTEX_POINT('',#13801);
#5083=VERTEX_POINT('',#13804);
#5084=VERTEX_POINT('',#13806);
#5085=VERTEX_POINT('',#13808);
#5086=VERTEX_POINT('',#13810);
#5087=VERTEX_POINT('',#13812);
#5088=VERTEX_POINT('',#13814);
#5089=VERTEX_POINT('',#13816);
#5090=VERTEX_POINT('',#13818);
#5091=VERTEX_POINT('',#13820);
#5092=VERTEX_POINT('',#13822);
#5093=VERTEX_POINT('',#13824);
#5094=VERTEX_POINT('',#13826);
#5095=VERTEX_POINT('',#13828);
#5096=VERTEX_POINT('',#13830);
#5097=VERTEX_POINT('',#13832);
#5098=VERTEX_POINT('',#13834);
#5099=VERTEX_POINT('',#13836);
#5100=VERTEX_POINT('',#13838);
#5101=VERTEX_POINT('',#13840);
#5102=VERTEX_POINT('',#13843);
#5103=VERTEX_POINT('',#13846);
#5104=VERTEX_POINT('',#13849);
#5105=VERTEX_POINT('',#13852);
#5106=VERTEX_POINT('',#13855);
#5107=VERTEX_POINT('',#13858);
#5108=VERTEX_POINT('',#13861);
#5109=VERTEX_POINT('',#13864);
#5110=VERTEX_POINT('',#13867);
#5111=VERTEX_POINT('',#13870);
#5112=VERTEX_POINT('',#13873);
#5113=VERTEX_POINT('',#13876);
#5114=VERTEX_POINT('',#13879);
#5115=VERTEX_POINT('',#13882);
#5116=VERTEX_POINT('',#13885);
#5117=VERTEX_POINT('',#13888);
#5118=VERTEX_POINT('',#13891);
#5119=VERTEX_POINT('',#13894);
#5120=VERTEX_POINT('',#13897);
#5121=VERTEX_POINT('',#13900);
#5122=VERTEX_POINT('',#13901);
#5123=VERTEX_POINT('',#13915);
#5124=VERTEX_POINT('',#13916);
#5125=VERTEX_POINT('',#13930);
#5126=VERTEX_POINT('',#13932);
#5127=VERTEX_POINT('',#13945);
#5128=VERTEX_POINT('',#13946);
#5129=VERTEX_POINT('',#13950);
#5130=VERTEX_POINT('',#13951);
#5131=VERTEX_POINT('',#13975);
#5132=VERTEX_POINT('',#13976);
#5133=VERTEX_POINT('',#13991);
#5134=VERTEX_POINT('',#14004);
#5135=VERTEX_POINT('',#14005);
#5136=VERTEX_POINT('',#14009);
#5137=VERTEX_POINT('',#14015);
#5138=VERTEX_POINT('',#14017);
#5139=VERTEX_POINT('',#14036);
#5140=VERTEX_POINT('',#14037);
#5141=VERTEX_POINT('',#14054);
#5142=VERTEX_POINT('',#14055);
#5143=VERTEX_POINT('',#14060);
#5144=VERTEX_POINT('',#14071);
#5145=VERTEX_POINT('',#14076);
#5146=VERTEX_POINT('',#14087);
#5147=VERTEX_POINT('',#14092);
#5148=VERTEX_POINT('',#14103);
#5149=VERTEX_POINT('',#14108);
#5150=VERTEX_POINT('',#14119);
#5151=VERTEX_POINT('',#14124);
#5152=VERTEX_POINT('',#14135);
#5153=VERTEX_POINT('',#14140);
#5154=VERTEX_POINT('',#14151);
#5155=VERTEX_POINT('',#14153);
#5156=VERTEX_POINT('',#14158);
#5157=VERTEX_POINT('',#14169);
#5158=VERTEX_POINT('',#14174);
#5159=VERTEX_POINT('',#14185);
#5160=VERTEX_POINT('',#14190);
#5161=VERTEX_POINT('',#14201);
#5162=VERTEX_POINT('',#14203);
#5163=VERTEX_POINT('',#14214);
#5164=VERTEX_POINT('',#14219);
#5165=VERTEX_POINT('',#14230);
#5166=VERTEX_POINT('',#14235);
#5167=VERTEX_POINT('',#14248);
#5168=VERTEX_POINT('',#14251);
#5169=VERTEX_POINT('',#14252);
#5170=VERTEX_POINT('',#14283);
#5171=VERTEX_POINT('',#14291);
#5172=VERTEX_POINT('',#14302);
#5173=VERTEX_POINT('',#14321);
#5174=VERTEX_POINT('',#14339);
#5175=VERTEX_POINT('',#14347);
#5176=VERTEX_POINT('',#14358);
#5177=VERTEX_POINT('',#14377);
#5178=VERTEX_POINT('',#14395);
#5179=VERTEX_POINT('',#14403);
#5180=VERTEX_POINT('',#14414);
#5181=VERTEX_POINT('',#14425);
#5182=VERTEX_POINT('',#14432);
#5183=VERTEX_POINT('',#14443);
#5184=VERTEX_POINT('',#14451);
#5185=VERTEX_POINT('',#14462);
#5186=VERTEX_POINT('',#14473);
#5187=VERTEX_POINT('',#14484);
#5188=VERTEX_POINT('',#14492);
#5189=VERTEX_POINT('',#14503);
#5190=VERTEX_POINT('',#14514);
#5191=VERTEX_POINT('',#14525);
#5192=VERTEX_POINT('',#14533);
#5193=VERTEX_POINT('',#14546);
#5194=VERTEX_POINT('',#14552);
#5195=VERTEX_POINT('',#14557);
#5196=VERTEX_POINT('',#14561);
#5197=VERTEX_POINT('',#14566);
#5198=VERTEX_POINT('',#14570);
#5199=VERTEX_POINT('',#14575);
#5200=VERTEX_POINT('',#14576);
#5201=VERTEX_POINT('',#14579);
#5202=VERTEX_POINT('',#14584);
#5203=VERTEX_POINT('',#14586);
#5204=VERTEX_POINT('',#14588);
#5205=VERTEX_POINT('',#14590);
#5206=VERTEX_POINT('',#14595);
#5207=VERTEX_POINT('',#14598);
#5208=VERTEX_POINT('',#14603);
#5209=VERTEX_POINT('',#14605);
#5210=VERTEX_POINT('',#14607);
#5211=VERTEX_POINT('',#14609);
#5212=VERTEX_POINT('',#14614);
#5213=VERTEX_POINT('',#14620);
#5214=VERTEX_POINT('',#14622);
#5215=VERTEX_POINT('',#14624);
#5216=VERTEX_POINT('',#14626);
#5217=VERTEX_POINT('',#14631);
#5218=VERTEX_POINT('',#14634);
#5219=VERTEX_POINT('',#14639);
#5220=VERTEX_POINT('',#14641);
#5221=VERTEX_POINT('',#14643);
#5222=VERTEX_POINT('',#14645);
#5223=VERTEX_POINT('',#14650);
#5224=VERTEX_POINT('',#14653);
#5225=VERTEX_POINT('',#14658);
#5226=VERTEX_POINT('',#14660);
#5227=VERTEX_POINT('',#14662);
#5228=VERTEX_POINT('',#14664);
#5229=VERTEX_POINT('',#14669);
#5230=VERTEX_POINT('',#14672);
#5231=VERTEX_POINT('',#14677);
#5232=VERTEX_POINT('',#14679);
#5233=VERTEX_POINT('',#14681);
#5234=VERTEX_POINT('',#14684);
#5235=VERTEX_POINT('',#14686);
#5236=VERTEX_POINT('',#14688);
#5237=VERTEX_POINT('',#14690);
#5238=VERTEX_POINT('',#14692);
#5239=VERTEX_POINT('',#14694);
#5240=VERTEX_POINT('',#14696);
#5241=VERTEX_POINT('',#14698);
#5242=VERTEX_POINT('',#14700);
#5243=VERTEX_POINT('',#14702);
#5244=VERTEX_POINT('',#14704);
#5245=VERTEX_POINT('',#14706);
#5246=VERTEX_POINT('',#14708);
#5247=VERTEX_POINT('',#14710);
#5248=VERTEX_POINT('',#14712);
#5249=VERTEX_POINT('',#14714);
#5250=VERTEX_POINT('',#14716);
#5251=VERTEX_POINT('',#14718);
#5252=VERTEX_POINT('',#14724);
#5253=VERTEX_POINT('',#14726);
#5254=VERTEX_POINT('',#14736);
#5255=VERTEX_POINT('',#14740);
#5256=VERTEX_POINT('',#14750);
#5257=VERTEX_POINT('',#14752);
#5258=VERTEX_POINT('',#14759);
#5259=VERTEX_POINT('',#14766);
#5260=VERTEX_POINT('',#14776);
#5261=VERTEX_POINT('',#14778);
#5262=VERTEX_POINT('',#14785);
#5263=VERTEX_POINT('',#14792);
#5264=VERTEX_POINT('',#14802);
#5265=VERTEX_POINT('',#14804);
#5266=VERTEX_POINT('',#14811);
#5267=VERTEX_POINT('',#14818);
#5268=VERTEX_POINT('',#14828);
#5269=VERTEX_POINT('',#14830);
#5270=VERTEX_POINT('',#14840);
#5271=VERTEX_POINT('',#14844);
#5272=VERTEX_POINT('',#14851);
#5273=VERTEX_POINT('',#14858);
#5274=VERTEX_POINT('',#14859);
#5275=VERTEX_POINT('',#14873);
#5276=VERTEX_POINT('',#14875);
#5277=VERTEX_POINT('',#14877);
#5278=VERTEX_POINT('',#14878);
#5279=VERTEX_POINT('',#14887);
#5280=VERTEX_POINT('',#14889);
#5281=VERTEX_POINT('',#14895);
#5282=VERTEX_POINT('',#14897);
#5283=VERTEX_POINT('',#14899);
#5284=VERTEX_POINT('',#14901);
#5285=VERTEX_POINT('',#14910);
#5286=VERTEX_POINT('',#14912);
#5287=VERTEX_POINT('',#14914);
#5288=VERTEX_POINT('',#14916);
#5289=VERTEX_POINT('',#14925);
#5290=VERTEX_POINT('',#14927);
#5291=VERTEX_POINT('',#14929);
#5292=VERTEX_POINT('',#14931);
#5293=VERTEX_POINT('',#14940);
#5294=VERTEX_POINT('',#14942);
#5295=VERTEX_POINT('',#14944);
#5296=VERTEX_POINT('',#14946);
#5297=VERTEX_POINT('',#14952);
#5298=VERTEX_POINT('',#14953);
#5299=VERTEX_POINT('',#14962);
#5300=VERTEX_POINT('',#14964);
#5301=VERTEX_POINT('',#14967);
#5302=VERTEX_POINT('',#14969);
#5303=VERTEX_POINT('',#14971);
#5304=VERTEX_POINT('',#14973);
#5305=VERTEX_POINT('',#14975);
#5306=VERTEX_POINT('',#14977);
#5307=VERTEX_POINT('',#14979);
#5308=VERTEX_POINT('',#14981);
#5309=VERTEX_POINT('',#14983);
#5310=VERTEX_POINT('',#14985);
#5311=VERTEX_POINT('',#14987);
#5312=VERTEX_POINT('',#14989);
#5313=VERTEX_POINT('',#14991);
#5314=VERTEX_POINT('',#14993);
#5315=VERTEX_POINT('',#14995);
#5316=VERTEX_POINT('',#14997);
#5317=VERTEX_POINT('',#14999);
#5318=VERTEX_POINT('',#15001);
#5319=VERTEX_POINT('',#15148);
#5320=VERTEX_POINT('',#15149);
#5321=VERTEX_POINT('',#15163);
#5322=VERTEX_POINT('',#15164);
#5323=VERTEX_POINT('',#15178);
#5324=VERTEX_POINT('',#15179);
#5325=VERTEX_POINT('',#15193);
#5326=VERTEX_POINT('',#15194);
#5327=VERTEX_POINT('',#15209);
#5328=VERTEX_POINT('',#15212);
#5329=VERTEX_POINT('',#15213);
#5330=VERTEX_POINT('',#15227);
#5331=VERTEX_POINT('',#15228);
#5332=VERTEX_POINT('',#15233);
#5333=VERTEX_POINT('',#15235);
#5334=VERTEX_POINT('',#15240);
#5335=VERTEX_POINT('',#15242);
#5336=VERTEX_POINT('',#15247);
#5337=VERTEX_POINT('',#15249);
#5338=VERTEX_POINT('',#15254);
#5339=VERTEX_POINT('',#15256);
#5340=VERTEX_POINT('',#15261);
#5341=VERTEX_POINT('',#15263);
#5342=VERTEX_POINT('',#15268);
#5343=VERTEX_POINT('',#15270);
#5344=VERTEX_POINT('',#15275);
#5345=VERTEX_POINT('',#15277);
#5346=VERTEX_POINT('',#15282);
#5347=VERTEX_POINT('',#15284);
#5348=VERTEX_POINT('',#15289);
#5349=VERTEX_POINT('',#15291);
#5350=VERTEX_POINT('',#15296);
#5351=VERTEX_POINT('',#15298);
#5352=VERTEX_POINT('',#15303);
#5353=VERTEX_POINT('',#15305);
#5354=VERTEX_POINT('',#15311);
#5355=VERTEX_POINT('',#15313);
#5356=VERTEX_POINT('',#15314);
#5357=VERTEX_POINT('',#15317);
#5358=VERTEX_POINT('',#15319);
#5359=VERTEX_POINT('',#15321);
#5360=VERTEX_POINT('',#15322);
#5361=VERTEX_POINT('',#15325);
#5362=VERTEX_POINT('',#15328);
#5363=VERTEX_POINT('',#15333);
#5364=VERTEX_POINT('',#15338);
#5365=VERTEX_POINT('',#15343);
#5366=VERTEX_POINT('',#15348);
#5367=VERTEX_POINT('',#15353);
#5368=VERTEX_POINT('',#15358);
#5369=VERTEX_POINT('',#15360);
#5370=VERTEX_POINT('',#15365);
#5371=VERTEX_POINT('',#15370);
#5372=VERTEX_POINT('',#15375);
#5373=VERTEX_POINT('',#15380);
#5374=VERTEX_POINT('',#15385);
#5375=VERTEX_POINT('',#15390);
#5376=VERTEX_POINT('',#15397);
#5377=VERTEX_POINT('',#15398);
#5378=VERTEX_POINT('',#15407);
#5379=VERTEX_POINT('',#15412);
#5380=VERTEX_POINT('',#15417);
#5381=VERTEX_POINT('',#15422);
#5382=VERTEX_POINT('',#15427);
#5383=VERTEX_POINT('',#15432);
#5384=VERTEX_POINT('',#15437);
#5385=VERTEX_POINT('',#15442);
#5386=VERTEX_POINT('',#15447);
#5387=VERTEX_POINT('',#15452);
#5388=VERTEX_POINT('',#15459);
#5389=VERTEX_POINT('',#15460);
#5390=VERTEX_POINT('',#15468);
#5391=VERTEX_POINT('',#15469);
#5392=VERTEX_POINT('',#15491);
#5393=VERTEX_POINT('',#15492);
#5394=VERTEX_POINT('',#15494);
#5395=VERTEX_POINT('',#15502);
#5396=VERTEX_POINT('',#15503);
#5397=VERTEX_POINT('',#15505);
#5398=VERTEX_POINT('',#15509);
#5399=VERTEX_POINT('',#15510);
#5400=VERTEX_POINT('',#15527);
#5401=VERTEX_POINT('',#15528);
#5402=VERTEX_POINT('',#15535);
#5403=VERTEX_POINT('',#15540);
#5404=VERTEX_POINT('',#15554);
#5405=VERTEX_POINT('',#15559);
#5406=VERTEX_POINT('',#15564);
#5407=VERTEX_POINT('',#15574);
#5408=VERTEX_POINT('',#15593);
#5409=VERTEX_POINT('',#15598);
#5410=VERTEX_POINT('',#15608);
#5411=VERTEX_POINT('',#15613);
#5412=VERTEX_POINT('',#15618);
#5413=VERTEX_POINT('',#15628);
#5414=VERTEX_POINT('',#15642);
#5415=VERTEX_POINT('',#15652);
#5416=VERTEX_POINT('',#15656);
#5417=VERTEX_POINT('',#15658);
#5418=VERTEX_POINT('',#15663);
#5419=VERTEX_POINT('',#15677);
#5420=VERTEX_POINT('',#15692);
#5421=VERTEX_POINT('',#15697);
#5422=VERTEX_POINT('',#15707);
#5423=VERTEX_POINT('',#15712);
#5424=VERTEX_POINT('',#15717);
#5425=VERTEX_POINT('',#15727);
#5426=VERTEX_POINT('',#15746);
#5427=VERTEX_POINT('',#15751);
#5428=VERTEX_POINT('',#15761);
#5429=VERTEX_POINT('',#15766);
#5430=VERTEX_POINT('',#15771);
#5431=VERTEX_POINT('',#15781);
#5432=VERTEX_POINT('',#15800);
#5433=VERTEX_POINT('',#15805);
#5434=VERTEX_POINT('',#15815);
#5435=VERTEX_POINT('',#15820);
#5436=VERTEX_POINT('',#15825);
#5437=VERTEX_POINT('',#15835);
#5438=VERTEX_POINT('',#15850);
#5439=VERTEX_POINT('',#15855);
#5440=VERTEX_POINT('',#15869);
#5441=VERTEX_POINT('',#15870);
#5442=VERTEX_POINT('',#15886);
#5443=VERTEX_POINT('',#15888);
#5444=VERTEX_POINT('',#15893);
#5445=VERTEX_POINT('',#15907);
#5446=VERTEX_POINT('',#15908);
#5447=VERTEX_POINT('',#15929);
#5448=VERTEX_POINT('',#15934);
#5449=VERTEX_POINT('',#15948);
#5450=VERTEX_POINT('',#15949);
#5451=VERTEX_POINT('',#15965);
#5452=VERTEX_POINT('',#15970);
#5453=VERTEX_POINT('',#15984);
#5454=VERTEX_POINT('',#15985);
#5455=VERTEX_POINT('',#16001);
#5456=VERTEX_POINT('',#16006);
#5457=VERTEX_POINT('',#16020);
#5458=VERTEX_POINT('',#16021);
#5459=VERTEX_POINT('',#16037);
#5460=VERTEX_POINT('',#16042);
#5461=VERTEX_POINT('',#16056);
#5462=VERTEX_POINT('',#16057);
#5463=VERTEX_POINT('',#16073);
#5464=VERTEX_POINT('',#16074);
#5465=VERTEX_POINT('',#16100);
#5466=VERTEX_POINT('',#16105);
#5467=VERTEX_POINT('',#16130);
#5468=VERTEX_POINT('',#16131);
#5469=VERTEX_POINT('',#16157);
#5470=VERTEX_POINT('',#16162);
#5471=VERTEX_POINT('',#16208);
#5472=VERTEX_POINT('',#16209);
#5473=VERTEX_POINT('',#16214);
#5474=VERTEX_POINT('',#16232);
#5475=VERTEX_POINT('',#16263);
#5476=VERTEX_POINT('',#16264);
#5477=VERTEX_POINT('',#16269);
#5478=VERTEX_POINT('',#16289);
#5479=VERTEX_POINT('',#16320);
#5480=VERTEX_POINT('',#16321);
#5481=VERTEX_POINT('',#16326);
#5482=VERTEX_POINT('',#16346);
#5483=VERTEX_POINT('',#16356);
#5484=VERTEX_POINT('',#16357);
#5485=VERTEX_POINT('',#16381);
#5486=VERTEX_POINT('',#16386);
#5487=VERTEX_POINT('',#16411);
#5488=VERTEX_POINT('',#16421);
#5489=VERTEX_POINT('',#16436);
#5490=VERTEX_POINT('',#16446);
#5491=VERTEX_POINT('',#16466);
#5492=VERTEX_POINT('',#16476);
#5493=VERTEX_POINT('',#16483);
#5494=VERTEX_POINT('',#16493);
#5495=VERTEX_POINT('',#16508);
#5496=VERTEX_POINT('',#16518);
#5497=VERTEX_POINT('',#16533);
#5498=VERTEX_POINT('',#16543);
#5499=CIRCLE('',#8241,0.0115);
#5500=CIRCLE('',#8242,0.0115);
#5501=CIRCLE('',#8244,0.0125);
#5502=CIRCLE('',#8246,0.016);
#5503=CIRCLE('',#8248,0.0125);
#5504=CIRCLE('',#8249,0.0125);
#5505=CIRCLE('',#8250,0.0125);
#5506=CIRCLE('',#8251,0.0125);
#5507=CIRCLE('',#8252,0.0125);
#5508=CIRCLE('',#8253,0.0125);
#5509=CIRCLE('',#8254,0.0125);
#5510=CIRCLE('',#8255,0.0125);
#5511=CIRCLE('',#8256,0.0125);
#5512=CIRCLE('',#8257,0.0125);
#5513=CIRCLE('',#8258,0.0125);
#5514=CIRCLE('',#8259,0.0125);
#5515=CIRCLE('',#8260,0.0125);
#5516=CIRCLE('',#8261,0.0125);
#5517=CIRCLE('',#8262,0.0125);
#5518=CIRCLE('',#8263,0.0125);
#5519=CIRCLE('',#8264,0.0125);
#5520=CIRCLE('',#8265,0.0125);
#5521=CIRCLE('',#8266,0.0125);
#5522=CIRCLE('',#8267,0.0125);
#5523=CIRCLE('',#8268,0.0125);
#5524=CIRCLE('',#8269,0.0125);
#5525=CIRCLE('',#8270,0.0125);
#5526=CIRCLE('',#8271,0.0125);
#5527=CIRCLE('',#8272,0.0125);
#5528=CIRCLE('',#8273,0.0125);
#5529=CIRCLE('',#8274,0.0125);
#5530=CIRCLE('',#8275,0.0125);
#5531=CIRCLE('',#8276,0.0125);
#5532=CIRCLE('',#8277,0.0125);
#5533=CIRCLE('',#8278,0.0125);
#5534=CIRCLE('',#8279,0.0125);
#5535=CIRCLE('',#8280,0.0125);
#5536=CIRCLE('',#8281,0.0125);
#5537=CIRCLE('',#8282,0.0125);
#5538=CIRCLE('',#8283,0.0125);
#5539=CIRCLE('',#8284,0.0125);
#5540=CIRCLE('',#8285,0.0125);
#5541=CIRCLE('',#8286,0.0125);
#5542=CIRCLE('',#8287,0.0125);
#5543=CIRCLE('',#8289,0.016);
#5544=CIRCLE('',#8291,0.013);
#5545=CIRCLE('',#8294,0.0175);
#5546=CIRCLE('',#8297,0.013);
#5547=CIRCLE('',#8300,0.0175);
#5548=CIRCLE('',#8303,0.013);
#5549=CIRCLE('',#8306,0.0175);
#5550=CIRCLE('',#8309,0.013);
#5551=CIRCLE('',#8312,0.0175);
#5552=CIRCLE('',#8315,0.013);
#5553=CIRCLE('',#8318,0.0175);
#5554=CIRCLE('',#8321,0.013);
#5555=CIRCLE('',#8324,0.0175);
#5556=CIRCLE('',#8327,0.013);
#5557=CIRCLE('',#8330,0.0175);
#5558=CIRCLE('',#8333,0.013);
#5559=CIRCLE('',#8336,0.0175);
#5560=CIRCLE('',#8339,0.013);
#5561=CIRCLE('',#8342,0.0175);
#5562=CIRCLE('',#8345,0.013);
#5563=CIRCLE('',#8348,0.0175);
#5564=CIRCLE('',#8351,0.013);
#5565=CIRCLE('',#8354,0.0175);
#5566=CIRCLE('',#8357,0.013);
#5567=CIRCLE('',#8360,0.0175);
#5568=CIRCLE('',#8363,0.013);
#5569=CIRCLE('',#8366,0.0175);
#5570=CIRCLE('',#8369,0.013);
#5571=CIRCLE('',#8372,0.0175);
#5572=CIRCLE('',#8375,0.013);
#5573=CIRCLE('',#8378,0.0175);
#5574=CIRCLE('',#8381,0.013);
#5575=CIRCLE('',#8384,0.0175);
#5576=CIRCLE('',#8387,0.013);
#5577=CIRCLE('',#8390,0.0175);
#5578=CIRCLE('',#8393,0.013);
#5579=CIRCLE('',#8396,0.0175);
#5580=CIRCLE('',#8399,0.013);
#5581=CIRCLE('',#8402,0.0175);
#5582=CIRCLE('',#8405,0.013);
#5583=CIRCLE('',#8408,0.0175);
#5584=CIRCLE('',#8411,0.0175);
#5585=CIRCLE('',#8413,0.013);
#5586=CIRCLE('',#8417,0.0175);
#5587=CIRCLE('',#8418,0.0175);
#5588=CIRCLE('',#8419,0.0175);
#5589=CIRCLE('',#8420,0.0175);
#5590=CIRCLE('',#8421,0.0175);
#5591=CIRCLE('',#8422,0.0175);
#5592=CIRCLE('',#8423,0.0175);
#5593=CIRCLE('',#8424,0.0175);
#5594=CIRCLE('',#8425,0.0175);
#5595=CIRCLE('',#8426,0.0175);
#5596=CIRCLE('',#8427,0.0175);
#5597=CIRCLE('',#8428,0.0175);
#5598=CIRCLE('',#8429,0.0175);
#5599=CIRCLE('',#8430,0.0175);
#5600=CIRCLE('',#8431,0.0175);
#5601=CIRCLE('',#8432,0.0175);
#5602=CIRCLE('',#8433,0.0175);
#5603=CIRCLE('',#8434,0.0175);
#5604=CIRCLE('',#8435,0.0175);
#5605=CIRCLE('',#8436,0.0175);
#5606=CIRCLE('',#8437,0.0175);
#5607=CIRCLE('',#8439,0.013);
#5608=CIRCLE('',#8443,0.013);
#5609=CIRCLE('',#8447,0.013);
#5610=CIRCLE('',#8451,0.013);
#5611=CIRCLE('',#8455,0.013);
#5612=CIRCLE('',#8459,0.013);
#5613=CIRCLE('',#8463,0.013);
#5614=CIRCLE('',#8467,0.013);
#5615=CIRCLE('',#8471,0.013);
#5616=CIRCLE('',#8475,0.013);
#5617=CIRCLE('',#8479,0.013);
#5618=CIRCLE('',#8483,0.013);
#5619=CIRCLE('',#8487,0.013);
#5620=CIRCLE('',#8491,0.013);
#5621=CIRCLE('',#8495,0.013);
#5622=CIRCLE('',#8499,0.013);
#5623=CIRCLE('',#8503,0.013);
#5624=CIRCLE('',#8507,0.013);
#5625=CIRCLE('',#8511,0.013);
#5626=CIRCLE('',#8515,0.0175);
#5627=CIRCLE('',#8519,0.0165);
#5628=CIRCLE('',#8539,0.0165);
#5629=CIRCLE('',#8543,0.0075);
#5630=CIRCLE('',#8544,0.0075);
#5631=CIRCLE('',#8546,0.00800000000055703);
#5632=CIRCLE('',#8548,0.012000000000557);
#5633=CIRCLE('',#8550,0.00850000000024656);
#5634=CIRCLE('',#8552,0.012000000000557);
#5635=CIRCLE('',#8554,0.0085);
#5636=CIRCLE('',#8556,0.00800000000055703);
#5637=CIRCLE('',#8558,0.00949999999944297);
#5638=CIRCLE('',#8560,0.008);
#5639=CIRCLE('',#8562,0.009);
#5640=CIRCLE('',#8565,0.00814644660912898);
#5641=CIRCLE('',#8567,0.009);
#5642=CIRCLE('',#8569,0.00835355339112897);
#5643=CIRCLE('',#8571,0.0085000000001643);
#5644=CIRCLE('',#8575,0.00850000000041746);
#5645=CIRCLE('',#8579,0.0075);
#5646=CIRCLE('',#8580,0.0075);
#5647=CIRCLE('',#8582,0.00800000000055703);
#5648=CIRCLE('',#8584,0.011000000000557);
#5649=CIRCLE('',#8586,0.00850000000024656);
#5650=CIRCLE('',#8588,0.011000000000557);
#5651=CIRCLE('',#8590,0.0085);
#5652=CIRCLE('',#8592,0.00800000000055703);
#5653=CIRCLE('',#8594,0.00949999999944297);
#5654=CIRCLE('',#8596,0.008);
#5655=CIRCLE('',#8598,0.009);
#5656=CIRCLE('',#8601,0.00814644660912898);
#5657=CIRCLE('',#8603,0.009);
#5658=CIRCLE('',#8605,0.00835355339112897);
#5659=CIRCLE('',#8607,0.0085000000001643);
#5660=CIRCLE('',#8611,0.00850000000041746);
#5661=CIRCLE('',#8615,0.0120000000003955);
#5662=CIRCLE('',#8616,0.0117000000001921);
#5663=CIRCLE('',#8618,0.01065);
#5664=CIRCLE('',#8620,0.012);
#5665=CIRCLE('',#8622,0.0106499999992724);
#5666=CIRCLE('',#8624,0.0117000000001921);
#5667=CIRCLE('',#8627,0.00842500000016944);
#5668=CIRCLE('',#8629,0.011075);
#5669=CIRCLE('',#8631,0.008425);
#5670=CIRCLE('',#8633,0.0110749999998306);
#5671=CIRCLE('',#8635,0.00779999999980785);
#5672=CIRCLE('',#8636,0.00779999999980785);
#5673=CIRCLE('',#8639,0.00885000000072759);
#5674=CIRCLE('',#8642,0.00749999999960454);
#5675=CIRCLE('',#8644,0.00885);
#5676=CIRCLE('',#8646,0.00749999999960454);
#5677=CIRCLE('',#8648,0.00779999999980785);
#5678=CIRCLE('',#8649,0.00779999999980785);
#5679=CIRCLE('',#8654,0.0120000000003955);
#5680=CIRCLE('',#8655,0.0117000000001921);
#5681=CIRCLE('',#8657,0.01065);
#5682=CIRCLE('',#8659,0.012);
#5683=CIRCLE('',#8661,0.0106499999992724);
#5684=CIRCLE('',#8663,0.0117000000001921);
#5685=CIRCLE('',#8666,0.00842500000016944);
#5686=CIRCLE('',#8668,0.011075);
#5687=CIRCLE('',#8670,0.008425);
#5688=CIRCLE('',#8672,0.0110749999998306);
#5689=CIRCLE('',#8674,0.00779999999980785);
#5690=CIRCLE('',#8675,0.00779999999980785);
#5691=CIRCLE('',#8678,0.00885000000072759);
#5692=CIRCLE('',#8681,0.00749999999960454);
#5693=CIRCLE('',#8683,0.00885);
#5694=CIRCLE('',#8685,0.00749999999960454);
#5695=CIRCLE('',#8687,0.00779999999980785);
#5696=CIRCLE('',#8688,0.00779999999980785);
#5697=CIRCLE('',#8693,0.016);
#5698=CIRCLE('',#8694,0.016);
#5699=CIRCLE('',#8696,0.01635);
#5700=CIRCLE('',#8698,0.01635);
#5701=CIRCLE('',#8700,0.01635);
#5702=CIRCLE('',#8702,0.01635);
#5703=CIRCLE('',#8704,0.016);
#5704=CIRCLE('',#8706,0.016);
#5705=CIRCLE('',#8708,0.016);
#5706=CIRCLE('',#8710,0.016);
#5707=CIRCLE('',#8712,0.01635);
#5708=CIRCLE('',#8714,0.01635);
#5709=CIRCLE('',#8716,0.01635);
#5710=CIRCLE('',#8718,0.01635);
#5711=CIRCLE('',#8720,0.016);
#5712=CIRCLE('',#8722,0.016);
#5713=CIRCLE('',#8724,0.016);
#5714=CIRCLE('',#8726,0.016);
#5715=CIRCLE('',#8728,0.01635);
#5716=CIRCLE('',#8730,0.01635);
#5717=CIRCLE('',#8732,0.01635);
#5718=CIRCLE('',#8734,0.01635);
#5719=CIRCLE('',#8736,0.016);
#5720=CIRCLE('',#8738,0.016);
#5721=CIRCLE('',#8740,0.016);
#5722=CIRCLE('',#8742,0.016);
#5723=CIRCLE('',#8744,0.0175);
#5724=CIRCLE('',#8746,0.0125);
#5725=CIRCLE('',#8748,0.0175);
#5726=CIRCLE('',#8750,0.0125);
#5727=CIRCLE('',#8752,0.0185);
#5728=CIRCLE('',#8754,0.0115);
#5729=CIRCLE('',#8756,0.0185);
#5730=CIRCLE('',#8758,0.0114999999999814);
#5731=CIRCLE('',#8760,0.0330000000001318);
#5732=CIRCLE('',#8761,0.0013);
#5733=CIRCLE('',#8762,0.0013);
#5734=CIRCLE('',#8763,0.0013);
#5735=CIRCLE('',#8764,0.0013);
#5736=CIRCLE('',#8765,0.0013);
#5737=CIRCLE('',#8766,0.0013);
#5738=CIRCLE('',#8767,0.0013);
#5739=CIRCLE('',#8768,0.0013);
#5740=CIRCLE('',#8769,0.0013);
#5741=CIRCLE('',#8770,0.0013);
#5742=CIRCLE('',#8771,0.0013);
#5743=CIRCLE('',#8772,0.0013);
#5744=CIRCLE('',#8773,0.0013);
#5745=CIRCLE('',#8774,0.0013);
#5746=CIRCLE('',#8775,0.0013);
#5747=CIRCLE('',#8776,0.0013);
#5748=CIRCLE('',#8777,0.0013);
#5749=CIRCLE('',#8778,0.0013);
#5750=CIRCLE('',#8780,0.012);
#5751=CIRCLE('',#8782,0.0013);
#5752=CIRCLE('',#8784,0.0013);
#5753=CIRCLE('',#8786,0.0013);
#5754=CIRCLE('',#8788,0.0013);
#5755=CIRCLE('',#8790,0.0013);
#5756=CIRCLE('',#8792,0.0013);
#5757=CIRCLE('',#8794,0.0013);
#5758=CIRCLE('',#8796,0.0013);
#5759=CIRCLE('',#8798,0.0013);
#5760=CIRCLE('',#8800,0.0013);
#5761=CIRCLE('',#8802,0.0013);
#5762=CIRCLE('',#8804,0.0013);
#5763=CIRCLE('',#8806,0.0013);
#5764=CIRCLE('',#8808,0.0013);
#5765=CIRCLE('',#8810,0.0013);
#5766=CIRCLE('',#8812,0.0013);
#5767=CIRCLE('',#8814,0.0013);
#5768=CIRCLE('',#8816,0.0013);
#5769=CIRCLE('',#8818,0.033999999999839);
#5770=CIRCLE('',#8820,0.0120000000000334);
#5771=CIRCLE('',#8822,0.0330000000001318);
#5772=CIRCLE('',#8823,0.0195);
#5773=CIRCLE('',#8825,0.034);
#5774=CIRCLE('',#8827,0.0115);
#5775=CIRCLE('',#8831,0.0115);
#5776=CIRCLE('',#8833,0.016303847577153);
#5777=CIRCLE('',#8835,0.0125);
#5778=CIRCLE('',#8837,0.016035898385);
#5779=CIRCLE('',#8840,0.0124999999996045);
#5780=CIRCLE('',#8842,0.016035898385);
#5781=CIRCLE('',#8843,0.016035898385);
#5782=CIRCLE('',#8845,0.0127999999998078);
#5783=CIRCLE('',#8847,0.017035898385);
#5784=CIRCLE('',#8850,0.0175358983831627);
#5785=CIRCLE('',#8855,0.0175358983842906);
#5786=CIRCLE('',#8860,0.0175358983832975);
#5787=CIRCLE('',#8863,0.00149999999977719);
#5788=CIRCLE('',#8867,0.0175358983831629);
#5789=CIRCLE('',#8872,0.0175358983842908);
#5790=CIRCLE('',#8877,0.0175358983832977);
#5791=CIRCLE('',#8880,0.0157358983850606);
#5792=CIRCLE('',#8882,0.017035898385);
#5793=CIRCLE('',#8884,0.0015);
#5794=CIRCLE('',#8885,0.0015);
#5795=CIRCLE('',#8887,0.0330000000001318);
#5796=CIRCLE('',#8888,0.0015);
#5797=CIRCLE('',#8889,0.0015);
#5798=CIRCLE('',#8890,0.0015);
#5799=CIRCLE('',#8891,0.024);
#5800=CIRCLE('',#8892,0.0015);
#5801=CIRCLE('',#8893,0.0015);
#5802=CIRCLE('',#8894,0.0015);
#5803=CIRCLE('',#8895,0.0015);
#5804=CIRCLE('',#8896,0.024);
#5805=CIRCLE('',#8897,0.0015);
#5806=CIRCLE('',#8898,0.0015);
#5807=CIRCLE('',#8899,0.0015);
#5808=CIRCLE('',#8900,0.024);
#5809=CIRCLE('',#8901,0.0015);
#5810=CIRCLE('',#8902,0.0015);
#5811=CIRCLE('',#8903,0.0015);
#5812=CIRCLE('',#8904,0.0015);
#5813=CIRCLE('',#8905,0.024);
#5814=CIRCLE('',#8906,0.0015);
#5815=CIRCLE('',#8907,0.0015);
#5816=CIRCLE('',#8908,0.0015);
#5817=CIRCLE('',#8909,0.0015);
#5818=CIRCLE('',#8910,0.024);
#5819=CIRCLE('',#8911,0.0015);
#5820=CIRCLE('',#8912,0.0015);
#5821=CIRCLE('',#8913,0.0015);
#5822=CIRCLE('',#8914,0.0015);
#5823=CIRCLE('',#8915,0.024);
#5824=CIRCLE('',#8916,0.0015);
#5825=CIRCLE('',#8917,0.0013);
#5826=CIRCLE('',#8918,0.0013);
#5827=CIRCLE('',#8919,0.0013);
#5828=CIRCLE('',#8920,0.0013);
#5829=CIRCLE('',#8921,0.0013);
#5830=CIRCLE('',#8922,0.0013);
#5831=CIRCLE('',#8923,0.0013);
#5832=CIRCLE('',#8924,0.0013);
#5833=CIRCLE('',#8925,0.0013);
#5834=CIRCLE('',#8926,0.0013);
#5835=CIRCLE('',#8927,0.0013);
#5836=CIRCLE('',#8928,0.0013);
#5837=CIRCLE('',#8929,0.0013);
#5838=CIRCLE('',#8930,0.0013);
#5839=CIRCLE('',#8931,0.0013);
#5840=CIRCLE('',#8932,0.0013);
#5841=CIRCLE('',#8933,0.0013);
#5842=CIRCLE('',#8934,0.0013);
#5843=CIRCLE('',#8936,0.0015);
#5844=CIRCLE('',#8938,0.017035898385);
#5845=CIRCLE('',#8940,0.0015);
#5846=CIRCLE('',#8942,0.0015);
#5847=CIRCLE('',#8944,0.017035898385);
#5848=CIRCLE('',#8946,0.0015);
#5849=CIRCLE('',#8948,0.0015);
#5850=CIRCLE('',#8950,0.017035898385);
#5851=CIRCLE('',#8952,0.0015);
#5852=CIRCLE('',#8954,0.0015);
#5853=CIRCLE('',#8956,0.017035898385);
#5854=CIRCLE('',#8958,0.0015);
#5855=CIRCLE('',#8960,0.0015);
#5856=CIRCLE('',#8962,0.017035898385);
#5857=CIRCLE('',#8964,0.0015);
#5858=CIRCLE('',#8966,0.0015);
#5859=CIRCLE('',#8968,0.0160358983845746);
#5860=CIRCLE('',#8970,0.0330000000001318);
#5861=CIRCLE('',#8971,0.0163358983848079);
#5862=CIRCLE('',#8972,0.0015);
#5863=CIRCLE('',#8973,0.0015);
#5864=CIRCLE('',#8974,0.024);
#5865=CIRCLE('',#8975,0.0015);
#5866=CIRCLE('',#8976,0.024);
#5867=CIRCLE('',#8977,0.0015);
#5868=CIRCLE('',#8978,0.0015);
#5869=CIRCLE('',#8979,0.024);
#5870=CIRCLE('',#8980,0.0015);
#5871=CIRCLE('',#8981,0.0015);
#5872=CIRCLE('',#8982,0.024);
#5873=CIRCLE('',#8983,0.0015);
#5874=CIRCLE('',#8984,0.0015);
#5875=CIRCLE('',#8985,0.024);
#5876=CIRCLE('',#8986,0.0015);
#5877=CIRCLE('',#8987,0.0015);
#5878=CIRCLE('',#8988,0.0015);
#5879=CIRCLE('',#8989,0.024);
#5880=CIRCLE('',#8990,0.0013);
#5881=CIRCLE('',#8991,0.0013);
#5882=CIRCLE('',#8992,0.0013);
#5883=CIRCLE('',#8993,0.0013);
#5884=CIRCLE('',#8994,0.0013);
#5885=CIRCLE('',#8995,0.0013);
#5886=CIRCLE('',#8996,0.0013);
#5887=CIRCLE('',#8997,0.0013);
#5888=CIRCLE('',#8998,0.0013);
#5889=CIRCLE('',#8999,0.0013);
#5890=CIRCLE('',#9000,0.0013);
#5891=CIRCLE('',#9001,0.0013);
#5892=CIRCLE('',#9002,0.0013);
#5893=CIRCLE('',#9003,0.0013);
#5894=CIRCLE('',#9004,0.0013);
#5895=CIRCLE('',#9005,0.0013);
#5896=CIRCLE('',#9006,0.0013);
#5897=CIRCLE('',#9007,0.0013);
#5898=CIRCLE('',#9057,0.033999999999839);
#5899=CIRCLE('',#9059,0.016035898385);
#5900=CIRCLE('',#9061,0.016035898385);
#5901=CIRCLE('',#9063,0.033999999999839);
#5902=CIRCLE('',#9066,0.0163358983848079);
#5903=CIRCLE('',#9068,0.016035898385);
#5904=CIRCLE('',#9070,0.016535898385);
#5905=CIRCLE('',#9071,0.0236999999709827);
#5906=CIRCLE('',#9072,0.016535898385);
#5907=CIRCLE('',#9073,0.023699999971322);
#5908=CIRCLE('',#9074,0.016535898385);
#5909=CIRCLE('',#9075,0.0236999999560649);
#5910=CIRCLE('',#9076,0.016535898385);
#5911=CIRCLE('',#9077,0.023699999970982);
#5912=CIRCLE('',#9078,0.016535898385);
#5913=CIRCLE('',#9079,0.0236999999713218);
#5914=CIRCLE('',#9080,0.016535898385);
#5915=CIRCLE('',#9081,0.0236999999852865);
#5916=CIRCLE('',#9082,0.00244999999960406);
#5917=CIRCLE('',#9083,0.00244999999980786);
#5918=CIRCLE('',#9084,0.00244999999980786);
#5919=CIRCLE('',#9085,0.00245000000014319);
#5920=CIRCLE('',#9086,0.00245000000014319);
#5921=CIRCLE('',#9087,0.00244999999980786);
#5922=CIRCLE('',#9088,0.00244999999980786);
#5923=CIRCLE('',#9089,0.00244999999960406);
#5924=CIRCLE('',#9091,0.00150000000045805);
#5925=CIRCLE('',#9092,0.0167858983853131);
#5926=CIRCLE('',#9093,0.00150000000045805);
#5927=CIRCLE('',#9096,0.00215000000003398);
#5928=CIRCLE('',#9098,0.00214999999960455);
#5929=CIRCLE('',#9101,0.00214999999988175);
#5930=CIRCLE('',#9102,0.00215000000003398);
#5931=CIRCLE('',#9104,0.00214999999988175);
#5932=CIRCLE('',#9105,0.00215000000003398);
#5933=CIRCLE('',#9107,0.00214999999960455);
#5934=CIRCLE('',#9109,0.00214999999960455);
#5935=CIRCLE('',#9111,0.00215000000003398);
#5936=CIRCLE('',#9121,0.000299999999290666);
#5937=CIRCLE('',#9123,0.000300000000142203);
#5938=CIRCLE('',#9124,0.0239999999561171);
#5939=CIRCLE('',#9141,0.0238500000003131);
#5940=CIRCLE('',#9162,0.024);
#5941=CIRCLE('',#9172,0.000299999999686457);
#5942=CIRCLE('',#9173,0.000300000000366869);
#5943=CIRCLE('',#9175,0.000299999999799668);
#5944=CIRCLE('',#9176,0.000299999999934399);
#5945=CIRCLE('',#9179,0.000300000000165203);
#5946=CIRCLE('',#9180,0.000299999999993383);
#5947=CIRCLE('',#9182,0.000299999999686456);
#5948=CIRCLE('',#9183,0.000300000000366864);
#5949=CIRCLE('',#9185,0.000299999999799668);
#5950=CIRCLE('',#9186,0.000299999999934399);
#5951=CIRCLE('',#9188,0.000300000000165203);
#5952=CIRCLE('',#9189,0.000299999999993381);
#5953=EDGE_LOOP('',(#1094));
#5954=EDGE_LOOP('',(#1095));
#5955=EDGE_LOOP('',(#1096));
#5956=EDGE_LOOP('',(#1097));
#5957=EDGE_LOOP('',(#1098));
#5958=EDGE_LOOP('',(#1099));
#5959=EDGE_LOOP('',(#1100));
#5960=EDGE_LOOP('',(#1101,#1102,#1103,#1104,#1105,#1106,#1107,#1108,#1109,
#1110,#1111,#1112,#1113,#1114,#1115,#1116,#1117,#1118,#1119,#1120,#1121,
#1122,#1123,#1124,#1125,#1126,#1127,#1128,#1129,#1130,#1131,#1132,#1133,
#1134,#1135,#1136,#1137,#1138,#1139,#1140,#1141,#1142,#1143,#1144,#1145,
#1146,#1147,#1148,#1149,#1150,#1151,#1152,#1153,#1154,#1155,#1156,#1157,
#1158,#1159,#1160,#1161,#1162,#1163,#1164,#1165,#1166,#1167,#1168,#1169,
#1170,#1171,#1172,#1173,#1174,#1175,#1176,#1177,#1178,#1179,#1180));
#5961=EDGE_LOOP('',(#1181));
#5962=EDGE_LOOP('',(#1182));
#5963=EDGE_LOOP('',(#1183,#1184,#1185,#1186));
#5964=EDGE_LOOP('',(#1187,#1188,#1189,#1190,#1191));
#5965=EDGE_LOOP('',(#1192,#1193,#1194,#1195,#1196,#1197));
#5966=EDGE_LOOP('',(#1198,#1199,#1200,#1201,#1202));
#5967=EDGE_LOOP('',(#1203,#1204,#1205,#1206));
#5968=EDGE_LOOP('',(#1207,#1208,#1209,#1210,#1211));
#5969=EDGE_LOOP('',(#1212,#1213,#1214,#1215,#1216,#1217));
#5970=EDGE_LOOP('',(#1218,#1219,#1220,#1221,#1222));
#5971=EDGE_LOOP('',(#1223,#1224,#1225,#1226));
#5972=EDGE_LOOP('',(#1227,#1228,#1229,#1230,#1231));
#5973=EDGE_LOOP('',(#1232,#1233,#1234,#1235,#1236,#1237));
#5974=EDGE_LOOP('',(#1238,#1239,#1240,#1241,#1242));
#5975=EDGE_LOOP('',(#1243,#1244,#1245,#1246));
#5976=EDGE_LOOP('',(#1247,#1248,#1249,#1250,#1251));
#5977=EDGE_LOOP('',(#1252,#1253,#1254,#1255,#1256,#1257));
#5978=EDGE_LOOP('',(#1258,#1259,#1260,#1261,#1262));
#5979=EDGE_LOOP('',(#1263,#1264,#1265,#1266));
#5980=EDGE_LOOP('',(#1267,#1268,#1269,#1270,#1271));
#5981=EDGE_LOOP('',(#1272,#1273,#1274,#1275,#1276,#1277));
#5982=EDGE_LOOP('',(#1278,#1279,#1280,#1281,#1282));
#5983=EDGE_LOOP('',(#1283,#1284,#1285,#1286));
#5984=EDGE_LOOP('',(#1287,#1288,#1289,#1290,#1291));
#5985=EDGE_LOOP('',(#1292,#1293,#1294,#1295,#1296,#1297));
#5986=EDGE_LOOP('',(#1298,#1299,#1300,#1301,#1302));
#5987=EDGE_LOOP('',(#1303,#1304,#1305,#1306));
#5988=EDGE_LOOP('',(#1307,#1308,#1309,#1310,#1311));
#5989=EDGE_LOOP('',(#1312,#1313,#1314,#1315,#1316,#1317));
#5990=EDGE_LOOP('',(#1318,#1319,#1320,#1321,#1322));
#5991=EDGE_LOOP('',(#1323,#1324,#1325,#1326));
#5992=EDGE_LOOP('',(#1327,#1328,#1329,#1330,#1331));
#5993=EDGE_LOOP('',(#1332,#1333,#1334,#1335,#1336,#1337));
#5994=EDGE_LOOP('',(#1338,#1339,#1340,#1341,#1342));
#5995=EDGE_LOOP('',(#1343,#1344,#1345,#1346));
#5996=EDGE_LOOP('',(#1347,#1348,#1349,#1350,#1351));
#5997=EDGE_LOOP('',(#1352,#1353,#1354,#1355,#1356,#1357));
#5998=EDGE_LOOP('',(#1358,#1359,#1360,#1361,#1362));
#5999=EDGE_LOOP('',(#1363,#1364,#1365,#1366));
#6000=EDGE_LOOP('',(#1367,#1368,#1369,#1370,#1371));
#6001=EDGE_LOOP('',(#1372,#1373,#1374,#1375,#1376,#1377));
#6002=EDGE_LOOP('',(#1378,#1379,#1380,#1381,#1382));
#6003=EDGE_LOOP('',(#1383,#1384,#1385,#1386));
#6004=EDGE_LOOP('',(#1387,#1388,#1389,#1390,#1391));
#6005=EDGE_LOOP('',(#1392,#1393,#1394,#1395,#1396,#1397));
#6006=EDGE_LOOP('',(#1398,#1399,#1400,#1401,#1402));
#6007=EDGE_LOOP('',(#1403,#1404,#1405,#1406));
#6008=EDGE_LOOP('',(#1407,#1408,#1409,#1410,#1411));
#6009=EDGE_LOOP('',(#1412,#1413,#1414,#1415,#1416,#1417));
#6010=EDGE_LOOP('',(#1418,#1419,#1420,#1421,#1422));
#6011=EDGE_LOOP('',(#1423,#1424,#1425,#1426));
#6012=EDGE_LOOP('',(#1427,#1428,#1429,#1430,#1431));
#6013=EDGE_LOOP('',(#1432,#1433,#1434,#1435,#1436,#1437));
#6014=EDGE_LOOP('',(#1438,#1439,#1440,#1441,#1442));
#6015=EDGE_LOOP('',(#1443,#1444,#1445,#1446));
#6016=EDGE_LOOP('',(#1447,#1448,#1449,#1450,#1451));
#6017=EDGE_LOOP('',(#1452,#1453,#1454,#1455,#1456,#1457));
#6018=EDGE_LOOP('',(#1458,#1459,#1460,#1461,#1462));
#6019=EDGE_LOOP('',(#1463,#1464,#1465,#1466));
#6020=EDGE_LOOP('',(#1467,#1468,#1469,#1470,#1471));
#6021=EDGE_LOOP('',(#1472,#1473,#1474,#1475,#1476,#1477));
#6022=EDGE_LOOP('',(#1478,#1479,#1480,#1481,#1482));
#6023=EDGE_LOOP('',(#1483,#1484,#1485,#1486));
#6024=EDGE_LOOP('',(#1487,#1488,#1489,#1490,#1491));
#6025=EDGE_LOOP('',(#1492,#1493,#1494,#1495,#1496,#1497));
#6026=EDGE_LOOP('',(#1498,#1499,#1500,#1501,#1502));
#6027=EDGE_LOOP('',(#1503,#1504,#1505,#1506));
#6028=EDGE_LOOP('',(#1507,#1508,#1509,#1510,#1511));
#6029=EDGE_LOOP('',(#1512,#1513,#1514,#1515,#1516,#1517));
#6030=EDGE_LOOP('',(#1518,#1519,#1520,#1521,#1522));
#6031=EDGE_LOOP('',(#1523,#1524,#1525,#1526));
#6032=EDGE_LOOP('',(#1527,#1528,#1529,#1530,#1531));
#6033=EDGE_LOOP('',(#1532,#1533,#1534,#1535,#1536,#1537));
#6034=EDGE_LOOP('',(#1538,#1539,#1540,#1541,#1542));
#6035=EDGE_LOOP('',(#1543,#1544,#1545,#1546));
#6036=EDGE_LOOP('',(#1547,#1548,#1549,#1550,#1551));
#6037=EDGE_LOOP('',(#1552,#1553,#1554,#1555,#1556,#1557));
#6038=EDGE_LOOP('',(#1558,#1559,#1560,#1561,#1562));
#6039=EDGE_LOOP('',(#1563,#1564,#1565,#1566));
#6040=EDGE_LOOP('',(#1567,#1568,#1569,#1570,#1571));
#6041=EDGE_LOOP('',(#1572,#1573,#1574,#1575,#1576,#1577));
#6042=EDGE_LOOP('',(#1578,#1579,#1580,#1581,#1582));
#6043=EDGE_LOOP('',(#1583));
#6044=EDGE_LOOP('',(#1584));
#6045=EDGE_LOOP('',(#1585,#1586,#1587,#1588));
#6046=EDGE_LOOP('',(#1589,#1590,#1591,#1592));
#6047=EDGE_LOOP('',(#1593,#1594,#1595,#1596));
#6048=EDGE_LOOP('',(#1597,#1598,#1599,#1600,#1601,#1602,#1603,#1604,#1605,
#1606,#1607,#1608,#1609,#1610,#1611,#1612,#1613,#1614,#1615,#1616,#1617,
#1618,#1619,#1620,#1621,#1622,#1623,#1624,#1625,#1626,#1627,#1628,#1629,
#1630,#1631,#1632,#1633,#1634,#1635,#1636,#1637,#1638,#1639,#1640,#1641,
#1642,#1643,#1644,#1645,#1646,#1647,#1648,#1649,#1650,#1651,#1652,#1653,
#1654,#1655,#1656,#1657,#1658,#1659,#1660,#1661,#1662,#1663,#1664,#1665,
#1666,#1667,#1668,#1669,#1670,#1671,#1672,#1673,#1674,#1675,#1676));
#6049=EDGE_LOOP('',(#1677));
#6050=EDGE_LOOP('',(#1678,#1679,#1680,#1681));
#6051=EDGE_LOOP('',(#1682,#1683,#1684,#1685));
#6052=EDGE_LOOP('',(#1686,#1687,#1688,#1689));
#6053=EDGE_LOOP('',(#1690,#1691,#1692,#1693));
#6054=EDGE_LOOP('',(#1694,#1695,#1696,#1697));
#6055=EDGE_LOOP('',(#1698,#1699,#1700,#1701));
#6056=EDGE_LOOP('',(#1702,#1703,#1704,#1705));
#6057=EDGE_LOOP('',(#1706,#1707,#1708,#1709));
#6058=EDGE_LOOP('',(#1710,#1711,#1712,#1713));
#6059=EDGE_LOOP('',(#1714,#1715,#1716,#1717));
#6060=EDGE_LOOP('',(#1718,#1719,#1720,#1721));
#6061=EDGE_LOOP('',(#1722,#1723,#1724,#1725));
#6062=EDGE_LOOP('',(#1726,#1727,#1728,#1729));
#6063=EDGE_LOOP('',(#1730,#1731,#1732,#1733));
#6064=EDGE_LOOP('',(#1734,#1735,#1736,#1737));
#6065=EDGE_LOOP('',(#1738,#1739,#1740,#1741));
#6066=EDGE_LOOP('',(#1742,#1743,#1744,#1745));
#6067=EDGE_LOOP('',(#1746,#1747,#1748,#1749));
#6068=EDGE_LOOP('',(#1750,#1751,#1752,#1753));
#6069=EDGE_LOOP('',(#1754,#1755,#1756,#1757));
#6070=EDGE_LOOP('',(#1758,#1759,#1760,#1761));
#6071=EDGE_LOOP('',(#1762,#1763,#1764,#1765));
#6072=EDGE_LOOP('',(#1766,#1767,#1768,#1769));
#6073=EDGE_LOOP('',(#1770,#1771,#1772,#1773));
#6074=EDGE_LOOP('',(#1774,#1775,#1776,#1777));
#6075=EDGE_LOOP('',(#1778,#1779,#1780,#1781));
#6076=EDGE_LOOP('',(#1782,#1783,#1784,#1785));
#6077=EDGE_LOOP('',(#1786,#1787,#1788,#1789));
#6078=EDGE_LOOP('',(#1790,#1791,#1792,#1793));
#6079=EDGE_LOOP('',(#1794,#1795,#1796,#1797));
#6080=EDGE_LOOP('',(#1798,#1799,#1800,#1801));
#6081=EDGE_LOOP('',(#1802,#1803,#1804,#1805));
#6082=EDGE_LOOP('',(#1806,#1807,#1808,#1809));
#6083=EDGE_LOOP('',(#1810,#1811,#1812,#1813));
#6084=EDGE_LOOP('',(#1814,#1815,#1816,#1817));
#6085=EDGE_LOOP('',(#1818,#1819,#1820,#1821));
#6086=EDGE_LOOP('',(#1822,#1823,#1824,#1825));
#6087=EDGE_LOOP('',(#1826,#1827,#1828,#1829));
#6088=EDGE_LOOP('',(#1830,#1831,#1832,#1833));
#6089=EDGE_LOOP('',(#1834,#1835,#1836,#1837));
#6090=EDGE_LOOP('',(#1838,#1839,#1840,#1841));
#6091=EDGE_LOOP('',(#1842,#1843,#1844,#1845));
#6092=EDGE_LOOP('',(#1846,#1847,#1848,#1849));
#6093=EDGE_LOOP('',(#1850,#1851,#1852,#1853));
#6094=EDGE_LOOP('',(#1854,#1855,#1856,#1857));
#6095=EDGE_LOOP('',(#1858,#1859,#1860,#1861));
#6096=EDGE_LOOP('',(#1862,#1863,#1864,#1865));
#6097=EDGE_LOOP('',(#1866,#1867,#1868,#1869));
#6098=EDGE_LOOP('',(#1870,#1871,#1872,#1873));
#6099=EDGE_LOOP('',(#1874,#1875,#1876,#1877));
#6100=EDGE_LOOP('',(#1878,#1879,#1880,#1881));
#6101=EDGE_LOOP('',(#1882,#1883,#1884,#1885));
#6102=EDGE_LOOP('',(#1886,#1887,#1888,#1889));
#6103=EDGE_LOOP('',(#1890,#1891,#1892,#1893));
#6104=EDGE_LOOP('',(#1894,#1895,#1896,#1897));
#6105=EDGE_LOOP('',(#1898,#1899,#1900,#1901));
#6106=EDGE_LOOP('',(#1902,#1903,#1904,#1905));
#6107=EDGE_LOOP('',(#1906));
#6108=EDGE_LOOP('',(#1907));
#6109=EDGE_LOOP('',(#1908,#1909,#1910,#1911));
#6110=EDGE_LOOP('',(#1912,#1913,#1914,#1915));
#6111=EDGE_LOOP('',(#1916));
#6112=EDGE_LOOP('',(#1917));
#6113=EDGE_LOOP('',(#1918,#1919,#1920,#1921));
#6114=EDGE_LOOP('',(#1922,#1923,#1924,#1925));
#6115=EDGE_LOOP('',(#1926,#1927,#1928,#1929));
#6116=EDGE_LOOP('',(#1930,#1931,#1932,#1933));
#6117=EDGE_LOOP('',(#1934,#1935,#1936,#1937));
#6118=EDGE_LOOP('',(#1938,#1939,#1940,#1941));
#6119=EDGE_LOOP('',(#1942,#1943,#1944,#1945));
#6120=EDGE_LOOP('',(#1946,#1947,#1948,#1949));
#6121=EDGE_LOOP('',(#1950,#1951,#1952,#1953));
#6122=EDGE_LOOP('',(#1954,#1955,#1956,#1957));
#6123=EDGE_LOOP('',(#1958,#1959,#1960,#1961));
#6124=EDGE_LOOP('',(#1962,#1963,#1964,#1965));
#6125=EDGE_LOOP('',(#1966,#1967,#1968,#1969));
#6126=EDGE_LOOP('',(#1970,#1971,#1972,#1973));
#6127=EDGE_LOOP('',(#1974,#1975,#1976,#1977));
#6128=EDGE_LOOP('',(#1978,#1979,#1980,#1981));
#6129=EDGE_LOOP('',(#1982,#1983,#1984,#1985));
#6130=EDGE_LOOP('',(#1986,#1987,#1988,#1989));
#6131=EDGE_LOOP('',(#1990));
#6132=EDGE_LOOP('',(#1991));
#6133=EDGE_LOOP('',(#1992));
#6134=EDGE_LOOP('',(#1993));
#6135=EDGE_LOOP('',(#1994));
#6136=EDGE_LOOP('',(#1995));
#6137=EDGE_LOOP('',(#1996));
#6138=EDGE_LOOP('',(#1997));
#6139=EDGE_LOOP('',(#1998));
#6140=EDGE_LOOP('',(#1999));
#6141=EDGE_LOOP('',(#2000,#2001));
#6142=EDGE_LOOP('',(#2002));
#6143=EDGE_LOOP('',(#2003));
#6144=EDGE_LOOP('',(#2004));
#6145=EDGE_LOOP('',(#2005,#2006));
#6146=EDGE_LOOP('',(#2007,#2008));
#6147=EDGE_LOOP('',(#2009,#2010));
#6148=EDGE_LOOP('',(#2011,#2012));
#6149=EDGE_LOOP('',(#2013));
#6150=EDGE_LOOP('',(#2014));
#6151=EDGE_LOOP('',(#2015,#2016));
#6152=EDGE_LOOP('',(#2017,#2018));
#6153=EDGE_LOOP('',(#2019,#2020));
#6154=EDGE_LOOP('',(#2021));
#6155=EDGE_LOOP('',(#2022,#2023,#2024,#2025));
#6156=EDGE_LOOP('',(#2026,#2027,#2028,#2029));
#6157=EDGE_LOOP('',(#2030,#2031));
#6158=EDGE_LOOP('',(#2032,#2033));
#6159=EDGE_LOOP('',(#2034,#2035));
#6160=EDGE_LOOP('',(#2036,#2037));
#6161=EDGE_LOOP('',(#2038,#2039,#2040,#2041));
#6162=EDGE_LOOP('',(#2042,#2043,#2044,#2045));
#6163=EDGE_LOOP('',(#2046,#2047,#2048,#2049));
#6164=EDGE_LOOP('',(#2050,#2051,#2052,#2053));
#6165=EDGE_LOOP('',(#2054,#2055));
#6166=EDGE_LOOP('',(#2056,#2057));
#6167=EDGE_LOOP('',(#2058));
#6168=EDGE_LOOP('',(#2059));
#6169=EDGE_LOOP('',(#2060));
#6170=EDGE_LOOP('',(#2061));
#6171=EDGE_LOOP('',(#2062));
#6172=EDGE_LOOP('',(#2063));
#6173=EDGE_LOOP('',(#2064,#2065));
#6174=EDGE_LOOP('',(#2066));
#6175=EDGE_LOOP('',(#2067));
#6176=EDGE_LOOP('',(#2068));
#6177=EDGE_LOOP('',(#2069,#2070));
#6178=EDGE_LOOP('',(#2071,#2072));
#6179=EDGE_LOOP('',(#2073,#2074));
#6180=EDGE_LOOP('',(#2075,#2076));
#6181=EDGE_LOOP('',(#2077));
#6182=EDGE_LOOP('',(#2078));
#6183=EDGE_LOOP('',(#2079,#2080));
#6184=EDGE_LOOP('',(#2081,#2082));
#6185=EDGE_LOOP('',(#2083,#2084));
#6186=EDGE_LOOP('',(#2085));
#6187=EDGE_LOOP('',(#2086,#2087,#2088,#2089));
#6188=EDGE_LOOP('',(#2090,#2091,#2092,#2093));
#6189=EDGE_LOOP('',(#2094,#2095));
#6190=EDGE_LOOP('',(#2096,#2097));
#6191=EDGE_LOOP('',(#2098,#2099));
#6192=EDGE_LOOP('',(#2100,#2101));
#6193=EDGE_LOOP('',(#2102,#2103,#2104,#2105));
#6194=EDGE_LOOP('',(#2106,#2107,#2108,#2109));
#6195=EDGE_LOOP('',(#2110,#2111,#2112,#2113));
#6196=EDGE_LOOP('',(#2114,#2115,#2116,#2117));
#6197=EDGE_LOOP('',(#2118,#2119));
#6198=EDGE_LOOP('',(#2120,#2121));
#6199=EDGE_LOOP('',(#2122,#2123));
#6200=EDGE_LOOP('',(#2124));
#6201=EDGE_LOOP('',(#2125));
#6202=EDGE_LOOP('',(#2126));
#6203=EDGE_LOOP('',(#2127,#2128));
#6204=EDGE_LOOP('',(#2129,#2130));
#6205=EDGE_LOOP('',(#2131));
#6206=EDGE_LOOP('',(#2132,#2133));
#6207=EDGE_LOOP('',(#2134));
#6208=EDGE_LOOP('',(#2135,#2136));
#6209=EDGE_LOOP('',(#2137,#2138,#2139,#2140));
#6210=EDGE_LOOP('',(#2141,#2142,#2143,#2144));
#6211=EDGE_LOOP('',(#2145));
#6212=EDGE_LOOP('',(#2146));
#6213=EDGE_LOOP('',(#2147,#2148));
#6214=EDGE_LOOP('',(#2149));
#6215=EDGE_LOOP('',(#2150,#2151));
#6216=EDGE_LOOP('',(#2152));
#6217=EDGE_LOOP('',(#2153));
#6218=EDGE_LOOP('',(#2154,#2155));
#6219=EDGE_LOOP('',(#2156,#2157,#2158,#2159));
#6220=EDGE_LOOP('',(#2160,#2161,#2162,#2163));
#6221=EDGE_LOOP('',(#2164,#2165,#2166,#2167));
#6222=EDGE_LOOP('',(#2168,#2169,#2170,#2171));
#6223=EDGE_LOOP('',(#2172));
#6224=EDGE_LOOP('',(#2173,#2174));
#6225=EDGE_LOOP('',(#2175,#2176));
#6226=EDGE_LOOP('',(#2177,#2178));
#6227=EDGE_LOOP('',(#2179));
#6228=EDGE_LOOP('',(#2180,#2181));
#6229=EDGE_LOOP('',(#2182,#2183,#2184,#2185));
#6230=EDGE_LOOP('',(#2186,#2187,#2188,#2189));
#6231=EDGE_LOOP('',(#2190,#2191));
#6232=EDGE_LOOP('',(#2192));
#6233=EDGE_LOOP('',(#2193));
#6234=EDGE_LOOP('',(#2194));
#6235=EDGE_LOOP('',(#2195,#2196));
#6236=EDGE_LOOP('',(#2197,#2198));
#6237=EDGE_LOOP('',(#2199));
#6238=EDGE_LOOP('',(#2200,#2201));
#6239=EDGE_LOOP('',(#2202));
#6240=EDGE_LOOP('',(#2203,#2204));
#6241=EDGE_LOOP('',(#2205,#2206,#2207,#2208));
#6242=EDGE_LOOP('',(#2209,#2210,#2211,#2212));
#6243=EDGE_LOOP('',(#2213));
#6244=EDGE_LOOP('',(#2214));
#6245=EDGE_LOOP('',(#2215,#2216));
#6246=EDGE_LOOP('',(#2217));
#6247=EDGE_LOOP('',(#2218,#2219));
#6248=EDGE_LOOP('',(#2220));
#6249=EDGE_LOOP('',(#2221));
#6250=EDGE_LOOP('',(#2222,#2223));
#6251=EDGE_LOOP('',(#2224,#2225,#2226,#2227));
#6252=EDGE_LOOP('',(#2228,#2229,#2230,#2231));
#6253=EDGE_LOOP('',(#2232,#2233,#2234,#2235));
#6254=EDGE_LOOP('',(#2236,#2237,#2238,#2239));
#6255=EDGE_LOOP('',(#2240));
#6256=EDGE_LOOP('',(#2241,#2242));
#6257=EDGE_LOOP('',(#2243,#2244));
#6258=EDGE_LOOP('',(#2245,#2246));
#6259=EDGE_LOOP('',(#2247));
#6260=EDGE_LOOP('',(#2248,#2249));
#6261=EDGE_LOOP('',(#2250,#2251,#2252,#2253));
#6262=EDGE_LOOP('',(#2254,#2255,#2256,#2257));
#6263=EDGE_LOOP('',(#2258));
#6264=EDGE_LOOP('',(#2259));
#6265=EDGE_LOOP('',(#2260));
#6266=EDGE_LOOP('',(#2261));
#6267=EDGE_LOOP('',(#2262));
#6268=EDGE_LOOP('',(#2263));
#6269=EDGE_LOOP('',(#2264));
#6270=EDGE_LOOP('',(#2265));
#6271=EDGE_LOOP('',(#2266));
#6272=EDGE_LOOP('',(#2267));
#6273=EDGE_LOOP('',(#2268));
#6274=EDGE_LOOP('',(#2269));
#6275=EDGE_LOOP('',(#2270));
#6276=EDGE_LOOP('',(#2271));
#6277=EDGE_LOOP('',(#2272));
#6278=EDGE_LOOP('',(#2273));
#6279=EDGE_LOOP('',(#2274));
#6280=EDGE_LOOP('',(#2275));
#6281=EDGE_LOOP('',(#2276));
#6282=EDGE_LOOP('',(#2277));
#6283=EDGE_LOOP('',(#2278));
#6284=EDGE_LOOP('',(#2279));
#6285=EDGE_LOOP('',(#2280));
#6286=EDGE_LOOP('',(#2281));
#6287=EDGE_LOOP('',(#2282));
#6288=EDGE_LOOP('',(#2283));
#6289=EDGE_LOOP('',(#2284));
#6290=EDGE_LOOP('',(#2285));
#6291=EDGE_LOOP('',(#2286));
#6292=EDGE_LOOP('',(#2287));
#6293=EDGE_LOOP('',(#2288));
#6294=EDGE_LOOP('',(#2289));
#6295=EDGE_LOOP('',(#2290));
#6296=EDGE_LOOP('',(#2291));
#6297=EDGE_LOOP('',(#2292));
#6298=EDGE_LOOP('',(#2293));
#6299=EDGE_LOOP('',(#2294));
#6300=EDGE_LOOP('',(#2295));
#6301=EDGE_LOOP('',(#2296));
#6302=EDGE_LOOP('',(#2297));
#6303=EDGE_LOOP('',(#2298));
#6304=EDGE_LOOP('',(#2299));
#6305=EDGE_LOOP('',(#2300));
#6306=EDGE_LOOP('',(#2301));
#6307=EDGE_LOOP('',(#2302));
#6308=EDGE_LOOP('',(#2303));
#6309=EDGE_LOOP('',(#2304));
#6310=EDGE_LOOP('',(#2305));
#6311=EDGE_LOOP('',(#2306));
#6312=EDGE_LOOP('',(#2307));
#6313=EDGE_LOOP('',(#2308));
#6314=EDGE_LOOP('',(#2309));
#6315=EDGE_LOOP('',(#2310));
#6316=EDGE_LOOP('',(#2311));
#6317=EDGE_LOOP('',(#2312));
#6318=EDGE_LOOP('',(#2313));
#6319=EDGE_LOOP('',(#2314));
#6320=EDGE_LOOP('',(#2315));
#6321=EDGE_LOOP('',(#2316));
#6322=EDGE_LOOP('',(#2317));
#6323=EDGE_LOOP('',(#2318));
#6324=EDGE_LOOP('',(#2319));
#6325=EDGE_LOOP('',(#2320));
#6326=EDGE_LOOP('',(#2321));
#6327=EDGE_LOOP('',(#2322));
#6328=EDGE_LOOP('',(#2323));
#6329=EDGE_LOOP('',(#2324));
#6330=EDGE_LOOP('',(#2325));
#6331=EDGE_LOOP('',(#2326));
#6332=EDGE_LOOP('',(#2327));
#6333=EDGE_LOOP('',(#2328));
#6334=EDGE_LOOP('',(#2329));
#6335=EDGE_LOOP('',(#2330));
#6336=EDGE_LOOP('',(#2331));
#6337=EDGE_LOOP('',(#2332));
#6338=EDGE_LOOP('',(#2333));
#6339=EDGE_LOOP('',(#2334));
#6340=EDGE_LOOP('',(#2335));
#6341=EDGE_LOOP('',(#2336));
#6342=EDGE_LOOP('',(#2337));
#6343=EDGE_LOOP('',(#2338));
#6344=EDGE_LOOP('',(#2339));
#6345=EDGE_LOOP('',(#2340));
#6346=EDGE_LOOP('',(#2341));
#6347=EDGE_LOOP('',(#2342));
#6348=EDGE_LOOP('',(#2343));
#6349=EDGE_LOOP('',(#2344));
#6350=EDGE_LOOP('',(#2345));
#6351=EDGE_LOOP('',(#2346));
#6352=EDGE_LOOP('',(#2347));
#6353=EDGE_LOOP('',(#2348));
#6354=EDGE_LOOP('',(#2349));
#6355=EDGE_LOOP('',(#2350));
#6356=EDGE_LOOP('',(#2351));
#6357=EDGE_LOOP('',(#2352));
#6358=EDGE_LOOP('',(#2353));
#6359=EDGE_LOOP('',(#2354));
#6360=EDGE_LOOP('',(#2355));
#6361=EDGE_LOOP('',(#2356));
#6362=EDGE_LOOP('',(#2357));
#6363=EDGE_LOOP('',(#2358));
#6364=EDGE_LOOP('',(#2359));
#6365=EDGE_LOOP('',(#2360));
#6366=EDGE_LOOP('',(#2361));
#6367=EDGE_LOOP('',(#2362));
#6368=EDGE_LOOP('',(#2363));
#6369=EDGE_LOOP('',(#2364));
#6370=EDGE_LOOP('',(#2365));
#6371=EDGE_LOOP('',(#2366));
#6372=EDGE_LOOP('',(#2367));
#6373=EDGE_LOOP('',(#2368));
#6374=EDGE_LOOP('',(#2369));
#6375=EDGE_LOOP('',(#2370));
#6376=EDGE_LOOP('',(#2371));
#6377=EDGE_LOOP('',(#2372));
#6378=EDGE_LOOP('',(#2373));
#6379=EDGE_LOOP('',(#2374));
#6380=EDGE_LOOP('',(#2375));
#6381=EDGE_LOOP('',(#2376));
#6382=EDGE_LOOP('',(#2377));
#6383=EDGE_LOOP('',(#2378));
#6384=EDGE_LOOP('',(#2379));
#6385=EDGE_LOOP('',(#2380));
#6386=EDGE_LOOP('',(#2381));
#6387=EDGE_LOOP('',(#2382,#2383));
#6388=EDGE_LOOP('',(#2384));
#6389=EDGE_LOOP('',(#2385));
#6390=EDGE_LOOP('',(#2386,#2387));
#6391=EDGE_LOOP('',(#2388));
#6392=EDGE_LOOP('',(#2389));
#6393=EDGE_LOOP('',(#2390));
#6394=EDGE_LOOP('',(#2391));
#6395=EDGE_LOOP('',(#2392));
#6396=EDGE_LOOP('',(#2393));
#6397=EDGE_LOOP('',(#2394));
#6398=EDGE_LOOP('',(#2395));
#6399=EDGE_LOOP('',(#2396));
#6400=EDGE_LOOP('',(#2397));
#6401=EDGE_LOOP('',(#2398));
#6402=EDGE_LOOP('',(#2399));
#6403=EDGE_LOOP('',(#2400));
#6404=EDGE_LOOP('',(#2401));
#6405=EDGE_LOOP('',(#2402));
#6406=EDGE_LOOP('',(#2403));
#6407=EDGE_LOOP('',(#2404));
#6408=EDGE_LOOP('',(#2405));
#6409=EDGE_LOOP('',(#2406));
#6410=EDGE_LOOP('',(#2407));
#6411=EDGE_LOOP('',(#2408,#2409));
#6412=EDGE_LOOP('',(#2410,#2411));
#6413=EDGE_LOOP('',(#2412,#2413));
#6414=EDGE_LOOP('',(#2414,#2415));
#6415=EDGE_LOOP('',(#2416));
#6416=EDGE_LOOP('',(#2417,#2418));
#6417=EDGE_LOOP('',(#2419,#2420));
#6418=EDGE_LOOP('',(#2421));
#6419=EDGE_LOOP('',(#2422,#2423));
#6420=EDGE_LOOP('',(#2424));
#6421=EDGE_LOOP('',(#2425,#2426));
#6422=EDGE_LOOP('',(#2427,#2428));
#6423=EDGE_LOOP('',(#2429));
#6424=EDGE_LOOP('',(#2430));
#6425=EDGE_LOOP('',(#2431,#2432,#2433,#2434));
#6426=EDGE_LOOP('',(#2435,#2436,#2437,#2438));
#6427=EDGE_LOOP('',(#2439,#2440));
#6428=EDGE_LOOP('',(#2441));
#6429=EDGE_LOOP('',(#2442,#2443));
#6430=EDGE_LOOP('',(#2444,#2445,#2446,#2447,#2448,#2449,#2450,#2451,#2452,
#2453,#2454,#2455,#2456,#2457,#2458,#2459,#2460,#2461,#2462,#2463,#2464,
#2465,#2466,#2467,#2468,#2469));
#6431=EDGE_LOOP('',(#2470,#2471));
#6432=EDGE_LOOP('',(#2472));
#6433=EDGE_LOOP('',(#2473,#2474,#2475,#2476,#2477));
#6434=EDGE_LOOP('',(#2478,#2479,#2480,#2481));
#6435=EDGE_LOOP('',(#2482,#2483,#2484,#2485));
#6436=EDGE_LOOP('',(#2486,#2487,#2488,#2489));
#6437=EDGE_LOOP('',(#2490,#2491,#2492,#2493));
#6438=EDGE_LOOP('',(#2494,#2495,#2496,#2497));
#6439=EDGE_LOOP('',(#2498,#2499,#2500,#2501));
#6440=EDGE_LOOP('',(#2502,#2503,#2504,#2505));
#6441=EDGE_LOOP('',(#2506,#2507,#2508,#2509));
#6442=EDGE_LOOP('',(#2510,#2511,#2512,#2513));
#6443=EDGE_LOOP('',(#2514,#2515,#2516,#2517));
#6444=EDGE_LOOP('',(#2518,#2519,#2520,#2521));
#6445=EDGE_LOOP('',(#2522,#2523,#2524,#2525));
#6446=EDGE_LOOP('',(#2526,#2527,#2528,#2529));
#6447=EDGE_LOOP('',(#2530,#2531,#2532,#2533));
#6448=EDGE_LOOP('',(#2534,#2535,#2536,#2537));
#6449=EDGE_LOOP('',(#2538,#2539,#2540,#2541));
#6450=EDGE_LOOP('',(#2542,#2543,#2544,#2545));
#6451=EDGE_LOOP('',(#2546,#2547,#2548,#2549));
#6452=EDGE_LOOP('',(#2550,#2551,#2552,#2553));
#6453=EDGE_LOOP('',(#2554,#2555,#2556,#2557));
#6454=EDGE_LOOP('',(#2558,#2559,#2560,#2561));
#6455=EDGE_LOOP('',(#2562,#2563,#2564,#2565));
#6456=EDGE_LOOP('',(#2566,#2567,#2568,#2569));
#6457=EDGE_LOOP('',(#2570,#2571,#2572,#2573));
#6458=EDGE_LOOP('',(#2574));
#6459=EDGE_LOOP('',(#2575));
#6460=EDGE_LOOP('',(#2576,#2577,#2578,#2579));
#6461=EDGE_LOOP('',(#2580,#2581,#2582,#2583,#2584));
#6462=EDGE_LOOP('',(#2585));
#6463=EDGE_LOOP('',(#2586,#2587,#2588,#2589,#2590,#2591,#2592,#2593,#2594,
#2595,#2596,#2597,#2598,#2599,#2600,#2601,#2602,#2603,#2604,#2605,#2606,
#2607,#2608,#2609,#2610,#2611,#2612,#2613,#2614,#2615,#2616,#2617,#2618,
#2619,#2620,#2621,#2622,#2623,#2624,#2625,#2626,#2627,#2628,#2629,#2630,
#2631,#2632,#2633));
#6464=EDGE_LOOP('',(#2634));
#6465=EDGE_LOOP('',(#2635));
#6466=EDGE_LOOP('',(#2636));
#6467=EDGE_LOOP('',(#2637));
#6468=EDGE_LOOP('',(#2638));
#6469=EDGE_LOOP('',(#2639));
#6470=EDGE_LOOP('',(#2640));
#6471=EDGE_LOOP('',(#2641));
#6472=EDGE_LOOP('',(#2642));
#6473=EDGE_LOOP('',(#2643));
#6474=EDGE_LOOP('',(#2644));
#6475=EDGE_LOOP('',(#2645));
#6476=EDGE_LOOP('',(#2646));
#6477=EDGE_LOOP('',(#2647));
#6478=EDGE_LOOP('',(#2648));
#6479=EDGE_LOOP('',(#2649));
#6480=EDGE_LOOP('',(#2650));
#6481=EDGE_LOOP('',(#2651));
#6482=EDGE_LOOP('',(#2652,#2653,#2654,#2655,#2656));
#6483=EDGE_LOOP('',(#2657,#2658,#2659,#2660));
#6484=EDGE_LOOP('',(#2661,#2662,#2663,#2664,#2665));
#6485=EDGE_LOOP('',(#2666,#2667,#2668,#2669,#2670));
#6486=EDGE_LOOP('',(#2671,#2672,#2673,#2674));
#6487=EDGE_LOOP('',(#2675,#2676,#2677,#2678,#2679));
#6488=EDGE_LOOP('',(#2680,#2681,#2682,#2683,#2684));
#6489=EDGE_LOOP('',(#2685,#2686,#2687,#2688,#2689));
#6490=EDGE_LOOP('',(#2690,#2691,#2692,#2693,#2694));
#6491=EDGE_LOOP('',(#2695,#2696,#2697,#2698,#2699));
#6492=EDGE_LOOP('',(#2700,#2701,#2702,#2703));
#6493=EDGE_LOOP('',(#2704,#2705,#2706,#2707,#2708));
#6494=EDGE_LOOP('',(#2709,#2710,#2711,#2712,#2713));
#6495=EDGE_LOOP('',(#2714,#2715,#2716,#2717));
#6496=EDGE_LOOP('',(#2718,#2719,#2720,#2721,#2722));
#6497=EDGE_LOOP('',(#2723,#2724,#2725,#2726,#2727));
#6498=EDGE_LOOP('',(#2728,#2729));
#6499=EDGE_LOOP('',(#2730));
#6500=EDGE_LOOP('',(#2731));
#6501=EDGE_LOOP('',(#2732));
#6502=EDGE_LOOP('',(#2733,#2734,#2735,#2736,#2737,#2738,#2739,#2740));
#6503=EDGE_LOOP('',(#2741,#2742,#2743,#2744,#2745,#2746,#2747,#2748));
#6504=EDGE_LOOP('',(#2749,#2750,#2751,#2752,#2753,#2754,#2755,#2756));
#6505=EDGE_LOOP('',(#2757,#2758,#2759,#2760,#2761,#2762,#2763,#2764));
#6506=EDGE_LOOP('',(#2765,#2766,#2767,#2768,#2769,#2770,#2771,#2772));
#6507=EDGE_LOOP('',(#2773,#2774,#2775,#2776,#2777,#2778,#2779,#2780));
#6508=EDGE_LOOP('',(#2781));
#6509=EDGE_LOOP('',(#2782));
#6510=EDGE_LOOP('',(#2783));
#6511=EDGE_LOOP('',(#2784));
#6512=EDGE_LOOP('',(#2785));
#6513=EDGE_LOOP('',(#2786));
#6514=EDGE_LOOP('',(#2787));
#6515=EDGE_LOOP('',(#2788));
#6516=EDGE_LOOP('',(#2789));
#6517=EDGE_LOOP('',(#2790));
#6518=EDGE_LOOP('',(#2791));
#6519=EDGE_LOOP('',(#2792));
#6520=EDGE_LOOP('',(#2793));
#6521=EDGE_LOOP('',(#2794));
#6522=EDGE_LOOP('',(#2795));
#6523=EDGE_LOOP('',(#2796));
#6524=EDGE_LOOP('',(#2797));
#6525=EDGE_LOOP('',(#2798));
#6526=EDGE_LOOP('',(#2799,#2800,#2801,#2802));
#6527=EDGE_LOOP('',(#2803));
#6528=EDGE_LOOP('',(#2804));
#6529=EDGE_LOOP('',(#2805));
#6530=EDGE_LOOP('',(#2806));
#6531=EDGE_LOOP('',(#2807));
#6532=EDGE_LOOP('',(#2808));
#6533=EDGE_LOOP('',(#2809));
#6534=EDGE_LOOP('',(#2810));
#6535=EDGE_LOOP('',(#2811));
#6536=EDGE_LOOP('',(#2812));
#6537=EDGE_LOOP('',(#2813));
#6538=EDGE_LOOP('',(#2814));
#6539=EDGE_LOOP('',(#2815));
#6540=EDGE_LOOP('',(#2816));
#6541=EDGE_LOOP('',(#2817));
#6542=EDGE_LOOP('',(#2818));
#6543=EDGE_LOOP('',(#2819));
#6544=EDGE_LOOP('',(#2820));
#6545=EDGE_LOOP('',(#2821));
#6546=EDGE_LOOP('',(#2822));
#6547=EDGE_LOOP('',(#2823));
#6548=EDGE_LOOP('',(#2824));
#6549=EDGE_LOOP('',(#2825));
#6550=EDGE_LOOP('',(#2826));
#6551=EDGE_LOOP('',(#2827));
#6552=EDGE_LOOP('',(#2828));
#6553=EDGE_LOOP('',(#2829));
#6554=EDGE_LOOP('',(#2830));
#6555=EDGE_LOOP('',(#2831));
#6556=EDGE_LOOP('',(#2832));
#6557=EDGE_LOOP('',(#2833));
#6558=EDGE_LOOP('',(#2834));
#6559=EDGE_LOOP('',(#2835));
#6560=EDGE_LOOP('',(#2836));
#6561=EDGE_LOOP('',(#2837));
#6562=EDGE_LOOP('',(#2838));
#6563=EDGE_LOOP('',(#2839,#2840,#2841,#2842));
#6564=EDGE_LOOP('',(#2843,#2844,#2845,#2846));
#6565=EDGE_LOOP('',(#2847,#2848,#2849,#2850));
#6566=EDGE_LOOP('',(#2851,#2852,#2853,#2854));
#6567=EDGE_LOOP('',(#2855,#2856,#2857,#2858));
#6568=EDGE_LOOP('',(#2859,#2860,#2861,#2862));
#6569=EDGE_LOOP('',(#2863,#2864,#2865,#2866));
#6570=EDGE_LOOP('',(#2867,#2868,#2869,#2870));
#6571=EDGE_LOOP('',(#2871,#2872,#2873,#2874));
#6572=EDGE_LOOP('',(#2875,#2876,#2877,#2878));
#6573=EDGE_LOOP('',(#2879,#2880,#2881,#2882));
#6574=EDGE_LOOP('',(#2883,#2884,#2885,#2886));
#6575=EDGE_LOOP('',(#2887,#2888,#2889,#2890));
#6576=EDGE_LOOP('',(#2891,#2892,#2893,#2894));
#6577=EDGE_LOOP('',(#2895,#2896,#2897,#2898));
#6578=EDGE_LOOP('',(#2899,#2900,#2901,#2902));
#6579=EDGE_LOOP('',(#2903,#2904,#2905,#2906));
#6580=EDGE_LOOP('',(#2907,#2908,#2909,#2910));
#6581=EDGE_LOOP('',(#2911,#2912,#2913,#2914));
#6582=EDGE_LOOP('',(#2915,#2916,#2917,#2918));
#6583=EDGE_LOOP('',(#2919,#2920,#2921,#2922));
#6584=EDGE_LOOP('',(#2923,#2924,#2925,#2926));
#6585=EDGE_LOOP('',(#2927,#2928,#2929,#2930));
#6586=EDGE_LOOP('',(#2931,#2932,#2933,#2934));
#6587=EDGE_LOOP('',(#2935,#2936,#2937,#2938));
#6588=EDGE_LOOP('',(#2939,#2940,#2941,#2942));
#6589=EDGE_LOOP('',(#2943,#2944,#2945,#2946));
#6590=EDGE_LOOP('',(#2947,#2948,#2949,#2950));
#6591=EDGE_LOOP('',(#2951,#2952,#2953,#2954));
#6592=EDGE_LOOP('',(#2955,#2956));
#6593=EDGE_LOOP('',(#2957));
#6594=EDGE_LOOP('',(#2958,#2959));
#6595=EDGE_LOOP('',(#2960,#2961));
#6596=EDGE_LOOP('',(#2962,#2963));
#6597=EDGE_LOOP('',(#2964));
#6598=EDGE_LOOP('',(#2965,#2966));
#6599=EDGE_LOOP('',(#2967));
#6600=EDGE_LOOP('',(#2968,#2969));
#6601=EDGE_LOOP('',(#2970,#2971));
#6602=EDGE_LOOP('',(#2972));
#6603=EDGE_LOOP('',(#2973,#2974));
#6604=EDGE_LOOP('',(#2975,#2976));
#6605=EDGE_LOOP('',(#2977,#2978));
#6606=EDGE_LOOP('',(#2979,#2980,#2981,#2982,#2983,#2984,#2985,#2986,#2987,
#2988,#2989,#2990,#2991,#2992,#2993,#2994,#2995,#2996,#2997,#2998,#2999,
#3000,#3001,#3002));
#6607=EDGE_LOOP('',(#3003));
#6608=EDGE_LOOP('',(#3004,#3005));
#6609=EDGE_LOOP('',(#3006));
#6610=EDGE_LOOP('',(#3007));
#6611=EDGE_LOOP('',(#3008,#3009));
#6612=EDGE_LOOP('',(#3010));
#6613=EDGE_LOOP('',(#3011));
#6614=EDGE_LOOP('',(#3012,#3013,#3014,#3015,#3016,#3017,#3018,#3019,#3020,
#3021,#3022,#3023,#3024,#3025,#3026,#3027));
#6615=EDGE_LOOP('',(#3028,#3029,#3030,#3031,#3032,#3033,#3034,#3035,#3036,
#3037,#3038,#3039,#3040,#3041,#3042,#3043));
#6616=EDGE_LOOP('',(#3044));
#6617=EDGE_LOOP('',(#3045,#3046));
#6618=EDGE_LOOP('',(#3047,#3048,#3049,#3050));
#6619=EDGE_LOOP('',(#3051,#3052,#3053,#3054));
#6620=EDGE_LOOP('',(#3055,#3056,#3057));
#6621=EDGE_LOOP('',(#3058));
#6622=EDGE_LOOP('',(#3059,#3060,#3061));
#6623=EDGE_LOOP('',(#3062));
#6624=EDGE_LOOP('',(#3063,#3064,#3065,#3066));
#6625=EDGE_LOOP('',(#3067,#3068,#3069,#3070));
#6626=EDGE_LOOP('',(#3071,#3072));
#6627=EDGE_LOOP('',(#3073));
#6628=EDGE_LOOP('',(#3074,#3075,#3076,#3077,#3078,#3079));
#6629=EDGE_LOOP('',(#3080,#3081,#3082,#3083,#3084,#3085));
#6630=EDGE_LOOP('',(#3086,#3087,#3088,#3089,#3090,#3091));
#6631=EDGE_LOOP('',(#3092,#3093,#3094,#3095,#3096));
#6632=EDGE_LOOP('',(#3097,#3098,#3099,#3100,#3101,#3102));
#6633=EDGE_LOOP('',(#3103,#3104,#3105,#3106,#3107,#3108));
#6634=EDGE_LOOP('',(#3109,#3110,#3111,#3112,#3113,#3114));
#6635=EDGE_LOOP('',(#3115,#3116,#3117,#3118,#3119));
#6636=EDGE_LOOP('',(#3120,#3121,#3122,#3123));
#6637=EDGE_LOOP('',(#3124,#3125,#3126,#3127,#3128));
#6638=EDGE_LOOP('',(#3129,#3130,#3131,#3132,#3133,#3134));
#6639=EDGE_LOOP('',(#3135,#3136,#3137,#3138));
#6640=EDGE_LOOP('',(#3139,#3140,#3141,#3142,#3143,#3144));
#6641=EDGE_LOOP('',(#3145,#3146,#3147,#3148,#3149,#3150));
#6642=EDGE_LOOP('',(#3151,#3152,#3153,#3154,#3155,#3156));
#6643=EDGE_LOOP('',(#3157,#3158,#3159,#3160,#3161));
#6644=EDGE_LOOP('',(#3162,#3163,#3164,#3165,#3166,#3167));
#6645=EDGE_LOOP('',(#3168,#3169,#3170,#3171,#3172,#3173));
#6646=EDGE_LOOP('',(#3174,#3175,#3176,#3177,#3178,#3179));
#6647=EDGE_LOOP('',(#3180,#3181,#3182,#3183));
#6648=EDGE_LOOP('',(#3184,#3185,#3186,#3187,#3188,#3189));
#6649=EDGE_LOOP('',(#3190,#3191,#3192,#3193,#3194,#3195));
#6650=EDGE_LOOP('',(#3196,#3197,#3198,#3199,#3200,#3201));
#6651=EDGE_LOOP('',(#3202,#3203,#3204,#3205));
#6652=EDGE_LOOP('',(#3206,#3207,#3208,#3209,#3210,#3211));
#6653=EDGE_LOOP('',(#3212,#3213));
#6654=EDGE_LOOP('',(#3214,#3215,#3216,#3217,#3218,#3219));
#6655=EDGE_LOOP('',(#3220,#3221));
#6656=EDGE_LOOP('',(#3222,#3223,#3224,#3225,#3226));
#6657=EDGE_LOOP('',(#3227,#3228,#3229,#3230,#3231,#3232));
#6658=EDGE_LOOP('',(#3233,#3234));
#6659=EDGE_LOOP('',(#3235,#3236,#3237,#3238,#3239,#3240));
#6660=EDGE_LOOP('',(#3241,#3242));
#6661=EDGE_LOOP('',(#3243,#3244,#3245,#3246,#3247,#3248));
#6662=EDGE_LOOP('',(#3249,#3250));
#6663=EDGE_LOOP('',(#3251,#3252,#3253,#3254,#3255,#3256));
#6664=EDGE_LOOP('',(#3257,#3258));
#6665=EDGE_LOOP('',(#3259,#3260,#3261,#3262));
#6666=EDGE_LOOP('',(#3263,#3264));
#6667=EDGE_LOOP('',(#3265,#3266,#3267,#3268));
#6668=EDGE_LOOP('',(#3269,#3270));
#6669=EDGE_LOOP('',(#3271,#3272,#3273));
#6670=EDGE_LOOP('',(#3274,#3275,#3276,#3277));
#6671=EDGE_LOOP('',(#3278,#3279,#3280));
#6672=EDGE_LOOP('',(#3281,#3282,#3283,#3284));
#6673=EDGE_LOOP('',(#3285,#3286));
#6674=EDGE_LOOP('',(#3287,#3288,#3289,#3290));
#6675=EDGE_LOOP('',(#3291,#3292,#3293,#3294));
#6676=EDGE_LOOP('',(#3295,#3296));
#6677=EDGE_LOOP('',(#3297,#3298,#3299,#3300,#3301));
#6678=EDGE_LOOP('',(#3302,#3303,#3304,#3305,#3306));
#6679=EDGE_LOOP('',(#3307,#3308,#3309,#3310));
#6680=EDGE_LOOP('',(#3311,#3312,#3313,#3314,#3315));
#6681=EDGE_LOOP('',(#3316,#3317,#3318,#3319,#3320));
#6682=EDGE_LOOP('',(#3321,#3322,#3323,#3324));
#6683=EDGE_LOOP('',(#3325,#3326,#3327));
#6684=EDGE_LOOP('',(#3328,#3329,#3330,#3331,#3332));
#6685=EDGE_LOOP('',(#3333,#3334,#3335,#3336));
#6686=EDGE_LOOP('',(#3337,#3338,#3339,#3340,#3341));
#6687=EDGE_LOOP('',(#3342,#3343,#3344,#3345,#3346));
#6688=EDGE_LOOP('',(#3347,#3348,#3349,#3350));
#6689=EDGE_LOOP('',(#3351,#3352,#3353,#3354,#3355));
#6690=EDGE_LOOP('',(#3356,#3357,#3358,#3359,#3360));
#6691=EDGE_LOOP('',(#3361,#3362,#3363,#3364));
#6692=EDGE_LOOP('',(#3365,#3366,#3367,#3368,#3369));
#6693=EDGE_LOOP('',(#3370,#3371,#3372,#3373,#3374));
#6694=EDGE_LOOP('',(#3375,#3376,#3377,#3378));
#6695=EDGE_LOOP('',(#3379,#3380,#3381,#3382,#3383));
#6696=EDGE_LOOP('',(#3384,#3385,#3386,#3387,#3388));
#6697=EDGE_LOOP('',(#3389,#3390,#3391,#3392));
#6698=EDGE_LOOP('',(#3393,#3394,#3395,#3396,#3397));
#6699=EDGE_LOOP('',(#3398,#3399,#3400,#3401,#3402));
#6700=EDGE_LOOP('',(#3403,#3404,#3405,#3406));
#6701=EDGE_LOOP('',(#3407,#3408,#3409,#3410,#3411));
#6702=EDGE_LOOP('',(#3412,#3413,#3414,#3415,#3416));
#6703=EDGE_LOOP('',(#3417,#3418,#3419,#3420,#3421));
#6704=EDGE_LOOP('',(#3422,#3423,#3424,#3425));
#6705=EDGE_LOOP('',(#3426,#3427,#3428,#3429,#3430));
#6706=EDGE_LOOP('',(#3431,#3432,#3433,#3434,#3435));
#6707=EDGE_LOOP('',(#3436,#3437,#3438,#3439));
#6708=EDGE_LOOP('',(#3440,#3441,#3442,#3443,#3444));
#6709=EDGE_LOOP('',(#3445,#3446,#3447,#3448,#3449));
#6710=EDGE_LOOP('',(#3450,#3451,#3452,#3453));
#6711=EDGE_LOOP('',(#3454,#3455,#3456,#3457,#3458));
#6712=EDGE_LOOP('',(#3459,#3460,#3461,#3462,#3463));
#6713=EDGE_LOOP('',(#3464,#3465,#3466,#3467));
#6714=FACE_BOUND('',#5953,.T.);
#6715=FACE_BOUND('',#5954,.T.);
#6716=FACE_BOUND('',#5955,.T.);
#6717=FACE_BOUND('',#5956,.T.);
#6718=FACE_BOUND('',#5957,.T.);
#6719=FACE_BOUND('',#5958,.T.);
#6720=FACE_BOUND('',#5959,.T.);
#6721=FACE_BOUND('',#5960,.T.);
#6722=FACE_BOUND('',#5961,.T.);
#6723=FACE_BOUND('',#5962,.T.);
#6724=FACE_BOUND('',#5963,.T.);
#6725=FACE_BOUND('',#5964,.T.);
#6726=FACE_BOUND('',#5965,.T.);
#6727=FACE_BOUND('',#5966,.T.);
#6728=FACE_BOUND('',#5967,.T.);
#6729=FACE_BOUND('',#5968,.T.);
#6730=FACE_BOUND('',#5969,.T.);
#6731=FACE_BOUND('',#5970,.T.);
#6732=FACE_BOUND('',#5971,.T.);
#6733=FACE_BOUND('',#5972,.T.);
#6734=FACE_BOUND('',#5973,.T.);
#6735=FACE_BOUND('',#5974,.T.);
#6736=FACE_BOUND('',#5975,.T.);
#6737=FACE_BOUND('',#5976,.T.);
#6738=FACE_BOUND('',#5977,.T.);
#6739=FACE_BOUND('',#5978,.T.);
#6740=FACE_BOUND('',#5979,.T.);
#6741=FACE_BOUND('',#5980,.T.);
#6742=FACE_BOUND('',#5981,.T.);
#6743=FACE_BOUND('',#5982,.T.);
#6744=FACE_BOUND('',#5983,.T.);
#6745=FACE_BOUND('',#5984,.T.);
#6746=FACE_BOUND('',#5985,.T.);
#6747=FACE_BOUND('',#5986,.T.);
#6748=FACE_BOUND('',#5987,.T.);
#6749=FACE_BOUND('',#5988,.T.);
#6750=FACE_BOUND('',#5989,.T.);
#6751=FACE_BOUND('',#5990,.T.);
#6752=FACE_BOUND('',#5991,.T.);
#6753=FACE_BOUND('',#5992,.T.);
#6754=FACE_BOUND('',#5993,.T.);
#6755=FACE_BOUND('',#5994,.T.);
#6756=FACE_BOUND('',#5995,.T.);
#6757=FACE_BOUND('',#5996,.T.);
#6758=FACE_BOUND('',#5997,.T.);
#6759=FACE_BOUND('',#5998,.T.);
#6760=FACE_BOUND('',#5999,.T.);
#6761=FACE_BOUND('',#6000,.T.);
#6762=FACE_BOUND('',#6001,.T.);
#6763=FACE_BOUND('',#6002,.T.);
#6764=FACE_BOUND('',#6003,.T.);
#6765=FACE_BOUND('',#6004,.T.);
#6766=FACE_BOUND('',#6005,.T.);
#6767=FACE_BOUND('',#6006,.T.);
#6768=FACE_BOUND('',#6007,.T.);
#6769=FACE_BOUND('',#6008,.T.);
#6770=FACE_BOUND('',#6009,.T.);
#6771=FACE_BOUND('',#6010,.T.);
#6772=FACE_BOUND('',#6011,.T.);
#6773=FACE_BOUND('',#6012,.T.);
#6774=FACE_BOUND('',#6013,.T.);
#6775=FACE_BOUND('',#6014,.T.);
#6776=FACE_BOUND('',#6015,.T.);
#6777=FACE_BOUND('',#6016,.T.);
#6778=FACE_BOUND('',#6017,.T.);
#6779=FACE_BOUND('',#6018,.T.);
#6780=FACE_BOUND('',#6019,.T.);
#6781=FACE_BOUND('',#6020,.T.);
#6782=FACE_BOUND('',#6021,.T.);
#6783=FACE_BOUND('',#6022,.T.);
#6784=FACE_BOUND('',#6023,.T.);
#6785=FACE_BOUND('',#6024,.T.);
#6786=FACE_BOUND('',#6025,.T.);
#6787=FACE_BOUND('',#6026,.T.);
#6788=FACE_BOUND('',#6027,.T.);
#6789=FACE_BOUND('',#6028,.T.);
#6790=FACE_BOUND('',#6029,.T.);
#6791=FACE_BOUND('',#6030,.T.);
#6792=FACE_BOUND('',#6031,.T.);
#6793=FACE_BOUND('',#6032,.T.);
#6794=FACE_BOUND('',#6033,.T.);
#6795=FACE_BOUND('',#6034,.T.);
#6796=FACE_BOUND('',#6035,.T.);
#6797=FACE_BOUND('',#6036,.T.);
#6798=FACE_BOUND('',#6037,.T.);
#6799=FACE_BOUND('',#6038,.T.);
#6800=FACE_BOUND('',#6039,.T.);
#6801=FACE_BOUND('',#6040,.T.);
#6802=FACE_BOUND('',#6041,.T.);
#6803=FACE_BOUND('',#6042,.T.);
#6804=FACE_BOUND('',#6043,.T.);
#6805=FACE_BOUND('',#6044,.T.);
#6806=FACE_BOUND('',#6045,.T.);
#6807=FACE_BOUND('',#6046,.T.);
#6808=FACE_BOUND('',#6047,.T.);
#6809=FACE_BOUND('',#6048,.T.);
#6810=FACE_BOUND('',#6049,.T.);
#6811=FACE_BOUND('',#6050,.T.);
#6812=FACE_BOUND('',#6051,.T.);
#6813=FACE_BOUND('',#6052,.T.);
#6814=FACE_BOUND('',#6053,.T.);
#6815=FACE_BOUND('',#6054,.T.);
#6816=FACE_BOUND('',#6055,.T.);
#6817=FACE_BOUND('',#6056,.T.);
#6818=FACE_BOUND('',#6057,.T.);
#6819=FACE_BOUND('',#6058,.T.);
#6820=FACE_BOUND('',#6059,.T.);
#6821=FACE_BOUND('',#6060,.T.);
#6822=FACE_BOUND('',#6061,.T.);
#6823=FACE_BOUND('',#6062,.T.);
#6824=FACE_BOUND('',#6063,.T.);
#6825=FACE_BOUND('',#6064,.T.);
#6826=FACE_BOUND('',#6065,.T.);
#6827=FACE_BOUND('',#6066,.T.);
#6828=FACE_BOUND('',#6067,.T.);
#6829=FACE_BOUND('',#6068,.T.);
#6830=FACE_BOUND('',#6069,.T.);
#6831=FACE_BOUND('',#6070,.T.);
#6832=FACE_BOUND('',#6071,.T.);
#6833=FACE_BOUND('',#6072,.T.);
#6834=FACE_BOUND('',#6073,.T.);
#6835=FACE_BOUND('',#6074,.T.);
#6836=FACE_BOUND('',#6075,.T.);
#6837=FACE_BOUND('',#6076,.T.);
#6838=FACE_BOUND('',#6077,.T.);
#6839=FACE_BOUND('',#6078,.T.);
#6840=FACE_BOUND('',#6079,.T.);
#6841=FACE_BOUND('',#6080,.T.);
#6842=FACE_BOUND('',#6081,.T.);
#6843=FACE_BOUND('',#6082,.T.);
#6844=FACE_BOUND('',#6083,.T.);
#6845=FACE_BOUND('',#6084,.T.);
#6846=FACE_BOUND('',#6085,.T.);
#6847=FACE_BOUND('',#6086,.T.);
#6848=FACE_BOUND('',#6087,.T.);
#6849=FACE_BOUND('',#6088,.T.);
#6850=FACE_BOUND('',#6089,.T.);
#6851=FACE_BOUND('',#6090,.T.);
#6852=FACE_BOUND('',#6091,.T.);
#6853=FACE_BOUND('',#6092,.T.);
#6854=FACE_BOUND('',#6093,.T.);
#6855=FACE_BOUND('',#6094,.T.);
#6856=FACE_BOUND('',#6095,.T.);
#6857=FACE_BOUND('',#6096,.T.);
#6858=FACE_BOUND('',#6097,.T.);
#6859=FACE_BOUND('',#6098,.T.);
#6860=FACE_BOUND('',#6099,.T.);
#6861=FACE_BOUND('',#6100,.T.);
#6862=FACE_BOUND('',#6101,.T.);
#6863=FACE_BOUND('',#6102,.T.);
#6864=FACE_BOUND('',#6103,.T.);
#6865=FACE_BOUND('',#6104,.T.);
#6866=FACE_BOUND('',#6105,.T.);
#6867=FACE_BOUND('',#6106,.T.);
#6868=FACE_BOUND('',#6107,.T.);
#6869=FACE_BOUND('',#6108,.T.);
#6870=FACE_BOUND('',#6109,.T.);
#6871=FACE_BOUND('',#6110,.T.);
#6872=FACE_BOUND('',#6111,.T.);
#6873=FACE_BOUND('',#6112,.T.);
#6874=FACE_BOUND('',#6113,.T.);
#6875=FACE_BOUND('',#6114,.T.);
#6876=FACE_BOUND('',#6115,.T.);
#6877=FACE_BOUND('',#6116,.T.);
#6878=FACE_BOUND('',#6117,.T.);
#6879=FACE_BOUND('',#6118,.T.);
#6880=FACE_BOUND('',#6119,.T.);
#6881=FACE_BOUND('',#6120,.T.);
#6882=FACE_BOUND('',#6121,.T.);
#6883=FACE_BOUND('',#6122,.T.);
#6884=FACE_BOUND('',#6123,.T.);
#6885=FACE_BOUND('',#6124,.T.);
#6886=FACE_BOUND('',#6125,.T.);
#6887=FACE_BOUND('',#6126,.T.);
#6888=FACE_BOUND('',#6127,.T.);
#6889=FACE_BOUND('',#6128,.T.);
#6890=FACE_BOUND('',#6129,.T.);
#6891=FACE_BOUND('',#6130,.T.);
#6892=FACE_BOUND('',#6131,.T.);
#6893=FACE_BOUND('',#6132,.T.);
#6894=FACE_BOUND('',#6133,.T.);
#6895=FACE_BOUND('',#6134,.T.);
#6896=FACE_BOUND('',#6135,.T.);
#6897=FACE_BOUND('',#6136,.T.);
#6898=FACE_BOUND('',#6137,.T.);
#6899=FACE_BOUND('',#6138,.T.);
#6900=FACE_BOUND('',#6139,.T.);
#6901=FACE_BOUND('',#6140,.T.);
#6902=FACE_BOUND('',#6141,.T.);
#6903=FACE_BOUND('',#6142,.T.);
#6904=FACE_BOUND('',#6143,.T.);
#6905=FACE_BOUND('',#6144,.T.);
#6906=FACE_BOUND('',#6145,.T.);
#6907=FACE_BOUND('',#6146,.T.);
#6908=FACE_BOUND('',#6147,.T.);
#6909=FACE_BOUND('',#6148,.T.);
#6910=FACE_BOUND('',#6149,.T.);
#6911=FACE_BOUND('',#6150,.T.);
#6912=FACE_BOUND('',#6151,.T.);
#6913=FACE_BOUND('',#6152,.T.);
#6914=FACE_BOUND('',#6153,.T.);
#6915=FACE_BOUND('',#6154,.T.);
#6916=FACE_BOUND('',#6155,.T.);
#6917=FACE_BOUND('',#6156,.T.);
#6918=FACE_BOUND('',#6157,.T.);
#6919=FACE_BOUND('',#6158,.T.);
#6920=FACE_BOUND('',#6159,.T.);
#6921=FACE_BOUND('',#6160,.T.);
#6922=FACE_BOUND('',#6161,.T.);
#6923=FACE_BOUND('',#6162,.T.);
#6924=FACE_BOUND('',#6163,.T.);
#6925=FACE_BOUND('',#6164,.T.);
#6926=FACE_BOUND('',#6165,.T.);
#6927=FACE_BOUND('',#6166,.T.);
#6928=FACE_BOUND('',#6167,.T.);
#6929=FACE_BOUND('',#6168,.T.);
#6930=FACE_BOUND('',#6169,.T.);
#6931=FACE_BOUND('',#6170,.T.);
#6932=FACE_BOUND('',#6171,.T.);
#6933=FACE_BOUND('',#6172,.T.);
#6934=FACE_BOUND('',#6173,.T.);
#6935=FACE_BOUND('',#6174,.T.);
#6936=FACE_BOUND('',#6175,.T.);
#6937=FACE_BOUND('',#6176,.T.);
#6938=FACE_BOUND('',#6177,.T.);
#6939=FACE_BOUND('',#6178,.T.);
#6940=FACE_BOUND('',#6179,.T.);
#6941=FACE_BOUND('',#6180,.T.);
#6942=FACE_BOUND('',#6181,.T.);
#6943=FACE_BOUND('',#6182,.T.);
#6944=FACE_BOUND('',#6183,.T.);
#6945=FACE_BOUND('',#6184,.T.);
#6946=FACE_BOUND('',#6185,.T.);
#6947=FACE_BOUND('',#6186,.T.);
#6948=FACE_BOUND('',#6187,.T.);
#6949=FACE_BOUND('',#6188,.T.);
#6950=FACE_BOUND('',#6189,.T.);
#6951=FACE_BOUND('',#6190,.T.);
#6952=FACE_BOUND('',#6191,.T.);
#6953=FACE_BOUND('',#6192,.T.);
#6954=FACE_BOUND('',#6193,.T.);
#6955=FACE_BOUND('',#6194,.T.);
#6956=FACE_BOUND('',#6195,.T.);
#6957=FACE_BOUND('',#6196,.T.);
#6958=FACE_BOUND('',#6197,.T.);
#6959=FACE_BOUND('',#6198,.T.);
#6960=FACE_BOUND('',#6199,.T.);
#6961=FACE_BOUND('',#6200,.T.);
#6962=FACE_BOUND('',#6201,.T.);
#6963=FACE_BOUND('',#6202,.T.);
#6964=FACE_BOUND('',#6203,.T.);
#6965=FACE_BOUND('',#6204,.T.);
#6966=FACE_BOUND('',#6205,.T.);
#6967=FACE_BOUND('',#6206,.T.);
#6968=FACE_BOUND('',#6207,.T.);
#6969=FACE_BOUND('',#6208,.T.);
#6970=FACE_BOUND('',#6209,.T.);
#6971=FACE_BOUND('',#6210,.T.);
#6972=FACE_BOUND('',#6211,.T.);
#6973=FACE_BOUND('',#6212,.T.);
#6974=FACE_BOUND('',#6213,.T.);
#6975=FACE_BOUND('',#6214,.T.);
#6976=FACE_BOUND('',#6215,.T.);
#6977=FACE_BOUND('',#6216,.T.);
#6978=FACE_BOUND('',#6217,.T.);
#6979=FACE_BOUND('',#6218,.T.);
#6980=FACE_BOUND('',#6219,.T.);
#6981=FACE_BOUND('',#6220,.T.);
#6982=FACE_BOUND('',#6221,.T.);
#6983=FACE_BOUND('',#6222,.T.);
#6984=FACE_BOUND('',#6223,.T.);
#6985=FACE_BOUND('',#6224,.T.);
#6986=FACE_BOUND('',#6225,.T.);
#6987=FACE_BOUND('',#6226,.T.);
#6988=FACE_BOUND('',#6227,.T.);
#6989=FACE_BOUND('',#6228,.T.);
#6990=FACE_BOUND('',#6229,.T.);
#6991=FACE_BOUND('',#6230,.T.);
#6992=FACE_BOUND('',#6231,.T.);
#6993=FACE_BOUND('',#6232,.T.);
#6994=FACE_BOUND('',#6233,.T.);
#6995=FACE_BOUND('',#6234,.T.);
#6996=FACE_BOUND('',#6235,.T.);
#6997=FACE_BOUND('',#6236,.T.);
#6998=FACE_BOUND('',#6237,.T.);
#6999=FACE_BOUND('',#6238,.T.);
#7000=FACE_BOUND('',#6239,.T.);
#7001=FACE_BOUND('',#6240,.T.);
#7002=FACE_BOUND('',#6241,.T.);
#7003=FACE_BOUND('',#6242,.T.);
#7004=FACE_BOUND('',#6243,.T.);
#7005=FACE_BOUND('',#6244,.T.);
#7006=FACE_BOUND('',#6245,.T.);
#7007=FACE_BOUND('',#6246,.T.);
#7008=FACE_BOUND('',#6247,.T.);
#7009=FACE_BOUND('',#6248,.T.);
#7010=FACE_BOUND('',#6249,.T.);
#7011=FACE_BOUND('',#6250,.T.);
#7012=FACE_BOUND('',#6251,.T.);
#7013=FACE_BOUND('',#6252,.T.);
#7014=FACE_BOUND('',#6253,.T.);
#7015=FACE_BOUND('',#6254,.T.);
#7016=FACE_BOUND('',#6255,.T.);
#7017=FACE_BOUND('',#6256,.T.);
#7018=FACE_BOUND('',#6257,.T.);
#7019=FACE_BOUND('',#6258,.T.);
#7020=FACE_BOUND('',#6259,.T.);
#7021=FACE_BOUND('',#6260,.T.);
#7022=FACE_BOUND('',#6261,.T.);
#7023=FACE_BOUND('',#6262,.T.);
#7024=FACE_BOUND('',#6263,.T.);
#7025=FACE_BOUND('',#6264,.T.);
#7026=FACE_BOUND('',#6265,.T.);
#7027=FACE_BOUND('',#6266,.T.);
#7028=FACE_BOUND('',#6267,.T.);
#7029=FACE_BOUND('',#6268,.T.);
#7030=FACE_BOUND('',#6269,.T.);
#7031=FACE_BOUND('',#6270,.T.);
#7032=FACE_BOUND('',#6271,.T.);
#7033=FACE_BOUND('',#6272,.T.);
#7034=FACE_BOUND('',#6273,.T.);
#7035=FACE_BOUND('',#6274,.T.);
#7036=FACE_BOUND('',#6275,.T.);
#7037=FACE_BOUND('',#6276,.T.);
#7038=FACE_BOUND('',#6277,.T.);
#7039=FACE_BOUND('',#6278,.T.);
#7040=FACE_BOUND('',#6279,.T.);
#7041=FACE_BOUND('',#6280,.T.);
#7042=FACE_BOUND('',#6281,.T.);
#7043=FACE_BOUND('',#6282,.T.);
#7044=FACE_BOUND('',#6283,.T.);
#7045=FACE_BOUND('',#6284,.T.);
#7046=FACE_BOUND('',#6285,.T.);
#7047=FACE_BOUND('',#6286,.T.);
#7048=FACE_BOUND('',#6287,.T.);
#7049=FACE_BOUND('',#6288,.T.);
#7050=FACE_BOUND('',#6289,.T.);
#7051=FACE_BOUND('',#6290,.T.);
#7052=FACE_BOUND('',#6291,.T.);
#7053=FACE_BOUND('',#6292,.T.);
#7054=FACE_BOUND('',#6293,.T.);
#7055=FACE_BOUND('',#6294,.T.);
#7056=FACE_BOUND('',#6295,.T.);
#7057=FACE_BOUND('',#6296,.T.);
#7058=FACE_BOUND('',#6297,.T.);
#7059=FACE_BOUND('',#6298,.T.);
#7060=FACE_BOUND('',#6299,.T.);
#7061=FACE_BOUND('',#6300,.T.);
#7062=FACE_BOUND('',#6301,.T.);
#7063=FACE_BOUND('',#6302,.T.);
#7064=FACE_BOUND('',#6303,.T.);
#7065=FACE_BOUND('',#6304,.T.);
#7066=FACE_BOUND('',#6305,.T.);
#7067=FACE_BOUND('',#6306,.T.);
#7068=FACE_BOUND('',#6307,.T.);
#7069=FACE_BOUND('',#6308,.T.);
#7070=FACE_BOUND('',#6309,.T.);
#7071=FACE_BOUND('',#6310,.T.);
#7072=FACE_BOUND('',#6311,.T.);
#7073=FACE_BOUND('',#6312,.T.);
#7074=FACE_BOUND('',#6313,.T.);
#7075=FACE_BOUND('',#6314,.T.);
#7076=FACE_BOUND('',#6315,.T.);
#7077=FACE_BOUND('',#6316,.T.);
#7078=FACE_BOUND('',#6317,.T.);
#7079=FACE_BOUND('',#6318,.T.);
#7080=FACE_BOUND('',#6319,.T.);
#7081=FACE_BOUND('',#6320,.T.);
#7082=FACE_BOUND('',#6321,.T.);
#7083=FACE_BOUND('',#6322,.T.);
#7084=FACE_BOUND('',#6323,.T.);
#7085=FACE_BOUND('',#6324,.T.);
#7086=FACE_BOUND('',#6325,.T.);
#7087=FACE_BOUND('',#6326,.T.);
#7088=FACE_BOUND('',#6327,.T.);
#7089=FACE_BOUND('',#6328,.T.);
#7090=FACE_BOUND('',#6329,.T.);
#7091=FACE_BOUND('',#6330,.T.);
#7092=FACE_BOUND('',#6331,.T.);
#7093=FACE_BOUND('',#6332,.T.);
#7094=FACE_BOUND('',#6333,.T.);
#7095=FACE_BOUND('',#6334,.T.);
#7096=FACE_BOUND('',#6335,.T.);
#7097=FACE_BOUND('',#6336,.T.);
#7098=FACE_BOUND('',#6337,.T.);
#7099=FACE_BOUND('',#6338,.T.);
#7100=FACE_BOUND('',#6339,.T.);
#7101=FACE_BOUND('',#6340,.T.);
#7102=FACE_BOUND('',#6341,.T.);
#7103=FACE_BOUND('',#6342,.T.);
#7104=FACE_BOUND('',#6343,.T.);
#7105=FACE_BOUND('',#6344,.T.);
#7106=FACE_BOUND('',#6345,.T.);
#7107=FACE_BOUND('',#6346,.T.);
#7108=FACE_BOUND('',#6347,.T.);
#7109=FACE_BOUND('',#6348,.T.);
#7110=FACE_BOUND('',#6349,.T.);
#7111=FACE_BOUND('',#6350,.T.);
#7112=FACE_BOUND('',#6351,.T.);
#7113=FACE_BOUND('',#6352,.T.);
#7114=FACE_BOUND('',#6353,.T.);
#7115=FACE_BOUND('',#6354,.T.);
#7116=FACE_BOUND('',#6355,.T.);
#7117=FACE_BOUND('',#6356,.T.);
#7118=FACE_BOUND('',#6357,.T.);
#7119=FACE_BOUND('',#6358,.T.);
#7120=FACE_BOUND('',#6359,.T.);
#7121=FACE_BOUND('',#6360,.T.);
#7122=FACE_BOUND('',#6361,.T.);
#7123=FACE_BOUND('',#6362,.T.);
#7124=FACE_BOUND('',#6363,.T.);
#7125=FACE_BOUND('',#6364,.T.);
#7126=FACE_BOUND('',#6365,.T.);
#7127=FACE_BOUND('',#6366,.T.);
#7128=FACE_BOUND('',#6367,.T.);
#7129=FACE_BOUND('',#6368,.T.);
#7130=FACE_BOUND('',#6369,.T.);
#7131=FACE_BOUND('',#6370,.T.);
#7132=FACE_BOUND('',#6371,.T.);
#7133=FACE_BOUND('',#6372,.T.);
#7134=FACE_BOUND('',#6373,.T.);
#7135=FACE_BOUND('',#6374,.T.);
#7136=FACE_BOUND('',#6375,.T.);
#7137=FACE_BOUND('',#6376,.T.);
#7138=FACE_BOUND('',#6377,.T.);
#7139=FACE_BOUND('',#6378,.T.);
#7140=FACE_BOUND('',#6379,.T.);
#7141=FACE_BOUND('',#6380,.T.);
#7142=FACE_BOUND('',#6381,.T.);
#7143=FACE_BOUND('',#6382,.T.);
#7144=FACE_BOUND('',#6383,.T.);
#7145=FACE_BOUND('',#6384,.T.);
#7146=FACE_BOUND('',#6385,.T.);
#7147=FACE_BOUND('',#6386,.T.);
#7148=FACE_BOUND('',#6387,.T.);
#7149=FACE_BOUND('',#6388,.T.);
#7150=FACE_BOUND('',#6389,.T.);
#7151=FACE_BOUND('',#6390,.T.);
#7152=FACE_BOUND('',#6391,.T.);
#7153=FACE_BOUND('',#6392,.T.);
#7154=FACE_BOUND('',#6393,.T.);
#7155=FACE_BOUND('',#6394,.T.);
#7156=FACE_BOUND('',#6395,.T.);
#7157=FACE_BOUND('',#6396,.T.);
#7158=FACE_BOUND('',#6397,.T.);
#7159=FACE_BOUND('',#6398,.T.);
#7160=FACE_BOUND('',#6399,.T.);
#7161=FACE_BOUND('',#6400,.T.);
#7162=FACE_BOUND('',#6401,.T.);
#7163=FACE_BOUND('',#6402,.T.);
#7164=FACE_BOUND('',#6403,.T.);
#7165=FACE_BOUND('',#6404,.T.);
#7166=FACE_BOUND('',#6405,.T.);
#7167=FACE_BOUND('',#6406,.T.);
#7168=FACE_BOUND('',#6407,.T.);
#7169=FACE_BOUND('',#6408,.T.);
#7170=FACE_BOUND('',#6409,.T.);
#7171=FACE_BOUND('',#6410,.T.);
#7172=FACE_BOUND('',#6411,.T.);
#7173=FACE_BOUND('',#6412,.T.);
#7174=FACE_BOUND('',#6413,.T.);
#7175=FACE_BOUND('',#6414,.T.);
#7176=FACE_BOUND('',#6415,.T.);
#7177=FACE_BOUND('',#6416,.T.);
#7178=FACE_BOUND('',#6417,.T.);
#7179=FACE_BOUND('',#6418,.T.);
#7180=FACE_BOUND('',#6419,.T.);
#7181=FACE_BOUND('',#6420,.T.);
#7182=FACE_BOUND('',#6421,.T.);
#7183=FACE_BOUND('',#6422,.T.);
#7184=FACE_BOUND('',#6423,.T.);
#7185=FACE_BOUND('',#6424,.T.);
#7186=FACE_BOUND('',#6425,.T.);
#7187=FACE_BOUND('',#6426,.T.);
#7188=FACE_BOUND('',#6427,.T.);
#7189=FACE_BOUND('',#6428,.T.);
#7190=FACE_BOUND('',#6429,.T.);
#7191=FACE_BOUND('',#6430,.T.);
#7192=FACE_BOUND('',#6431,.T.);
#7193=FACE_BOUND('',#6432,.T.);
#7194=FACE_BOUND('',#6433,.T.);
#7195=FACE_BOUND('',#6434,.T.);
#7196=FACE_BOUND('',#6435,.T.);
#7197=FACE_BOUND('',#6436,.T.);
#7198=FACE_BOUND('',#6437,.T.);
#7199=FACE_BOUND('',#6438,.T.);
#7200=FACE_BOUND('',#6439,.T.);
#7201=FACE_BOUND('',#6440,.T.);
#7202=FACE_BOUND('',#6441,.T.);
#7203=FACE_BOUND('',#6442,.T.);
#7204=FACE_BOUND('',#6443,.T.);
#7205=FACE_BOUND('',#6444,.T.);
#7206=FACE_BOUND('',#6445,.T.);
#7207=FACE_BOUND('',#6446,.T.);
#7208=FACE_BOUND('',#6447,.T.);
#7209=FACE_BOUND('',#6448,.T.);
#7210=FACE_BOUND('',#6449,.T.);
#7211=FACE_BOUND('',#6450,.T.);
#7212=FACE_BOUND('',#6451,.T.);
#7213=FACE_BOUND('',#6452,.T.);
#7214=FACE_BOUND('',#6453,.T.);
#7215=FACE_BOUND('',#6454,.T.);
#7216=FACE_BOUND('',#6455,.T.);
#7217=FACE_BOUND('',#6456,.T.);
#7218=FACE_BOUND('',#6457,.T.);
#7219=FACE_BOUND('',#6458,.T.);
#7220=FACE_BOUND('',#6459,.T.);
#7221=FACE_BOUND('',#6460,.T.);
#7222=FACE_BOUND('',#6461,.T.);
#7223=FACE_BOUND('',#6462,.T.);
#7224=FACE_BOUND('',#6463,.T.);
#7225=FACE_BOUND('',#6464,.T.);
#7226=FACE_BOUND('',#6465,.T.);
#7227=FACE_BOUND('',#6466,.T.);
#7228=FACE_BOUND('',#6467,.T.);
#7229=FACE_BOUND('',#6468,.T.);
#7230=FACE_BOUND('',#6469,.T.);
#7231=FACE_BOUND('',#6470,.T.);
#7232=FACE_BOUND('',#6471,.T.);
#7233=FACE_BOUND('',#6472,.T.);
#7234=FACE_BOUND('',#6473,.T.);
#7235=FACE_BOUND('',#6474,.T.);
#7236=FACE_BOUND('',#6475,.T.);
#7237=FACE_BOUND('',#6476,.T.);
#7238=FACE_BOUND('',#6477,.T.);
#7239=FACE_BOUND('',#6478,.T.);
#7240=FACE_BOUND('',#6479,.T.);
#7241=FACE_BOUND('',#6480,.T.);
#7242=FACE_BOUND('',#6481,.T.);
#7243=FACE_BOUND('',#6482,.T.);
#7244=FACE_BOUND('',#6483,.T.);
#7245=FACE_BOUND('',#6484,.T.);
#7246=FACE_BOUND('',#6485,.T.);
#7247=FACE_BOUND('',#6486,.T.);
#7248=FACE_BOUND('',#6487,.T.);
#7249=FACE_BOUND('',#6488,.T.);
#7250=FACE_BOUND('',#6489,.T.);
#7251=FACE_BOUND('',#6490,.T.);
#7252=FACE_BOUND('',#6491,.T.);
#7253=FACE_BOUND('',#6492,.T.);
#7254=FACE_BOUND('',#6493,.T.);
#7255=FACE_BOUND('',#6494,.T.);
#7256=FACE_BOUND('',#6495,.T.);
#7257=FACE_BOUND('',#6496,.T.);
#7258=FACE_BOUND('',#6497,.T.);
#7259=FACE_BOUND('',#6498,.T.);
#7260=FACE_BOUND('',#6499,.T.);
#7261=FACE_BOUND('',#6500,.T.);
#7262=FACE_BOUND('',#6501,.T.);
#7263=FACE_BOUND('',#6502,.T.);
#7264=FACE_BOUND('',#6503,.T.);
#7265=FACE_BOUND('',#6504,.T.);
#7266=FACE_BOUND('',#6505,.T.);
#7267=FACE_BOUND('',#6506,.T.);
#7268=FACE_BOUND('',#6507,.T.);
#7269=FACE_BOUND('',#6508,.T.);
#7270=FACE_BOUND('',#6509,.T.);
#7271=FACE_BOUND('',#6510,.T.);
#7272=FACE_BOUND('',#6511,.T.);
#7273=FACE_BOUND('',#6512,.T.);
#7274=FACE_BOUND('',#6513,.T.);
#7275=FACE_BOUND('',#6514,.T.);
#7276=FACE_BOUND('',#6515,.T.);
#7277=FACE_BOUND('',#6516,.T.);
#7278=FACE_BOUND('',#6517,.T.);
#7279=FACE_BOUND('',#6518,.T.);
#7280=FACE_BOUND('',#6519,.T.);
#7281=FACE_BOUND('',#6520,.T.);
#7282=FACE_BOUND('',#6521,.T.);
#7283=FACE_BOUND('',#6522,.T.);
#7284=FACE_BOUND('',#6523,.T.);
#7285=FACE_BOUND('',#6524,.T.);
#7286=FACE_BOUND('',#6525,.T.);
#7287=FACE_BOUND('',#6526,.T.);
#7288=FACE_BOUND('',#6527,.T.);
#7289=FACE_BOUND('',#6528,.T.);
#7290=FACE_BOUND('',#6529,.T.);
#7291=FACE_BOUND('',#6530,.T.);
#7292=FACE_BOUND('',#6531,.T.);
#7293=FACE_BOUND('',#6532,.T.);
#7294=FACE_BOUND('',#6533,.T.);
#7295=FACE_BOUND('',#6534,.T.);
#7296=FACE_BOUND('',#6535,.T.);
#7297=FACE_BOUND('',#6536,.T.);
#7298=FACE_BOUND('',#6537,.T.);
#7299=FACE_BOUND('',#6538,.T.);
#7300=FACE_BOUND('',#6539,.T.);
#7301=FACE_BOUND('',#6540,.T.);
#7302=FACE_BOUND('',#6541,.T.);
#7303=FACE_BOUND('',#6542,.T.);
#7304=FACE_BOUND('',#6543,.T.);
#7305=FACE_BOUND('',#6544,.T.);
#7306=FACE_BOUND('',#6545,.T.);
#7307=FACE_BOUND('',#6546,.T.);
#7308=FACE_BOUND('',#6547,.T.);
#7309=FACE_BOUND('',#6548,.T.);
#7310=FACE_BOUND('',#6549,.T.);
#7311=FACE_BOUND('',#6550,.T.);
#7312=FACE_BOUND('',#6551,.T.);
#7313=FACE_BOUND('',#6552,.T.);
#7314=FACE_BOUND('',#6553,.T.);
#7315=FACE_BOUND('',#6554,.T.);
#7316=FACE_BOUND('',#6555,.T.);
#7317=FACE_BOUND('',#6556,.T.);
#7318=FACE_BOUND('',#6557,.T.);
#7319=FACE_BOUND('',#6558,.T.);
#7320=FACE_BOUND('',#6559,.T.);
#7321=FACE_BOUND('',#6560,.T.);
#7322=FACE_BOUND('',#6561,.T.);
#7323=FACE_BOUND('',#6562,.T.);
#7324=FACE_BOUND('',#6563,.T.);
#7325=FACE_BOUND('',#6564,.T.);
#7326=FACE_BOUND('',#6565,.T.);
#7327=FACE_BOUND('',#6566,.T.);
#7328=FACE_BOUND('',#6567,.T.);
#7329=FACE_BOUND('',#6568,.T.);
#7330=FACE_BOUND('',#6569,.T.);
#7331=FACE_BOUND('',#6570,.T.);
#7332=FACE_BOUND('',#6571,.T.);
#7333=FACE_BOUND('',#6572,.T.);
#7334=FACE_BOUND('',#6573,.T.);
#7335=FACE_BOUND('',#6574,.T.);
#7336=FACE_BOUND('',#6575,.T.);
#7337=FACE_BOUND('',#6576,.T.);
#7338=FACE_BOUND('',#6577,.T.);
#7339=FACE_BOUND('',#6578,.T.);
#7340=FACE_BOUND('',#6579,.T.);
#7341=FACE_BOUND('',#6580,.T.);
#7342=FACE_BOUND('',#6581,.T.);
#7343=FACE_BOUND('',#6582,.T.);
#7344=FACE_BOUND('',#6583,.T.);
#7345=FACE_BOUND('',#6584,.T.);
#7346=FACE_BOUND('',#6585,.T.);
#7347=FACE_BOUND('',#6586,.T.);
#7348=FACE_BOUND('',#6587,.T.);
#7349=FACE_BOUND('',#6588,.T.);
#7350=FACE_BOUND('',#6589,.T.);
#7351=FACE_BOUND('',#6590,.T.);
#7352=FACE_BOUND('',#6591,.T.);
#7353=FACE_BOUND('',#6592,.T.);
#7354=FACE_BOUND('',#6593,.T.);
#7355=FACE_BOUND('',#6594,.T.);
#7356=FACE_BOUND('',#6595,.T.);
#7357=FACE_BOUND('',#6596,.T.);
#7358=FACE_BOUND('',#6597,.T.);
#7359=FACE_BOUND('',#6598,.T.);
#7360=FACE_BOUND('',#6599,.T.);
#7361=FACE_BOUND('',#6600,.T.);
#7362=FACE_BOUND('',#6601,.T.);
#7363=FACE_BOUND('',#6602,.T.);
#7364=FACE_BOUND('',#6603,.T.);
#7365=FACE_BOUND('',#6604,.T.);
#7366=FACE_BOUND('',#6605,.T.);
#7367=FACE_BOUND('',#6606,.T.);
#7368=FACE_BOUND('',#6607,.T.);
#7369=FACE_BOUND('',#6608,.T.);
#7370=FACE_BOUND('',#6609,.T.);
#7371=FACE_BOUND('',#6610,.T.);
#7372=FACE_BOUND('',#6611,.T.);
#7373=FACE_BOUND('',#6612,.T.);
#7374=FACE_BOUND('',#6613,.T.);
#7375=FACE_BOUND('',#6614,.T.);
#7376=FACE_BOUND('',#6615,.T.);
#7377=FACE_BOUND('',#6616,.T.);
#7378=FACE_BOUND('',#6617,.T.);
#7379=FACE_BOUND('',#6618,.T.);
#7380=FACE_BOUND('',#6619,.T.);
#7381=FACE_BOUND('',#6620,.T.);
#7382=FACE_BOUND('',#6621,.T.);
#7383=FACE_BOUND('',#6622,.T.);
#7384=FACE_BOUND('',#6623,.T.);
#7385=FACE_BOUND('',#6624,.T.);
#7386=FACE_BOUND('',#6625,.T.);
#7387=FACE_BOUND('',#6626,.T.);
#7388=FACE_BOUND('',#6627,.T.);
#7389=FACE_BOUND('',#6628,.T.);
#7390=FACE_BOUND('',#6629,.T.);
#7391=FACE_BOUND('',#6630,.T.);
#7392=FACE_BOUND('',#6631,.T.);
#7393=FACE_BOUND('',#6632,.T.);
#7394=FACE_BOUND('',#6633,.T.);
#7395=FACE_BOUND('',#6634,.T.);
#7396=FACE_BOUND('',#6635,.T.);
#7397=FACE_BOUND('',#6636,.T.);
#7398=FACE_BOUND('',#6637,.T.);
#7399=FACE_BOUND('',#6638,.T.);
#7400=FACE_BOUND('',#6639,.T.);
#7401=FACE_BOUND('',#6640,.T.);
#7402=FACE_BOUND('',#6641,.T.);
#7403=FACE_BOUND('',#6642,.T.);
#7404=FACE_BOUND('',#6643,.T.);
#7405=FACE_BOUND('',#6644,.T.);
#7406=FACE_BOUND('',#6645,.T.);
#7407=FACE_BOUND('',#6646,.T.);
#7408=FACE_BOUND('',#6647,.T.);
#7409=FACE_BOUND('',#6648,.T.);
#7410=FACE_BOUND('',#6649,.T.);
#7411=FACE_BOUND('',#6650,.T.);
#7412=FACE_BOUND('',#6651,.T.);
#7413=FACE_BOUND('',#6652,.T.);
#7414=FACE_BOUND('',#6653,.T.);
#7415=FACE_BOUND('',#6654,.T.);
#7416=FACE_BOUND('',#6655,.T.);
#7417=FACE_BOUND('',#6656,.T.);
#7418=FACE_BOUND('',#6657,.T.);
#7419=FACE_BOUND('',#6658,.T.);
#7420=FACE_BOUND('',#6659,.T.);
#7421=FACE_BOUND('',#6660,.T.);
#7422=FACE_BOUND('',#6661,.T.);
#7423=FACE_BOUND('',#6662,.T.);
#7424=FACE_BOUND('',#6663,.T.);
#7425=FACE_BOUND('',#6664,.T.);
#7426=FACE_BOUND('',#6665,.T.);
#7427=FACE_BOUND('',#6666,.T.);
#7428=FACE_BOUND('',#6667,.T.);
#7429=FACE_BOUND('',#6668,.T.);
#7430=FACE_BOUND('',#6669,.T.);
#7431=FACE_BOUND('',#6670,.T.);
#7432=FACE_BOUND('',#6671,.T.);
#7433=FACE_BOUND('',#6672,.T.);
#7434=FACE_BOUND('',#6673,.T.);
#7435=FACE_BOUND('',#6674,.T.);
#7436=FACE_BOUND('',#6675,.T.);
#7437=FACE_BOUND('',#6676,.T.);
#7438=FACE_BOUND('',#6677,.T.);
#7439=FACE_BOUND('',#6678,.T.);
#7440=FACE_BOUND('',#6679,.T.);
#7441=FACE_BOUND('',#6680,.T.);
#7442=FACE_BOUND('',#6681,.T.);
#7443=FACE_BOUND('',#6682,.T.);
#7444=FACE_BOUND('',#6683,.T.);
#7445=FACE_BOUND('',#6684,.T.);
#7446=FACE_BOUND('',#6685,.T.);
#7447=FACE_BOUND('',#6686,.T.);
#7448=FACE_BOUND('',#6687,.T.);
#7449=FACE_BOUND('',#6688,.T.);
#7450=FACE_BOUND('',#6689,.T.);
#7451=FACE_BOUND('',#6690,.T.);
#7452=FACE_BOUND('',#6691,.T.);
#7453=FACE_BOUND('',#6692,.T.);
#7454=FACE_BOUND('',#6693,.T.);
#7455=FACE_BOUND('',#6694,.T.);
#7456=FACE_BOUND('',#6695,.T.);
#7457=FACE_BOUND('',#6696,.T.);
#7458=FACE_BOUND('',#6697,.T.);
#7459=FACE_BOUND('',#6698,.T.);
#7460=FACE_BOUND('',#6699,.T.);
#7461=FACE_BOUND('',#6700,.T.);
#7462=FACE_BOUND('',#6701,.T.);
#7463=FACE_BOUND('',#6702,.T.);
#7464=FACE_BOUND('',#6703,.T.);
#7465=FACE_BOUND('',#6704,.T.);
#7466=FACE_BOUND('',#6705,.T.);
#7467=FACE_BOUND('',#6706,.T.);
#7468=FACE_BOUND('',#6707,.T.);
#7469=FACE_BOUND('',#6708,.T.);
#7470=FACE_BOUND('',#6709,.T.);
#7471=FACE_BOUND('',#6710,.T.);
#7472=FACE_BOUND('',#6711,.T.);
#7473=FACE_BOUND('',#6712,.T.);
#7474=FACE_BOUND('',#6713,.T.);
#7475=CYLINDRICAL_SURFACE('',#8240,0.0115);
#7476=CYLINDRICAL_SURFACE('',#8247,0.0125);
#7477=CYLINDRICAL_SURFACE('',#8288,0.016);
#7478=CYLINDRICAL_SURFACE('',#8412,0.013);
#7479=CYLINDRICAL_SURFACE('',#8416,0.0175);
#7480=CYLINDRICAL_SURFACE('',#8438,0.013);
#7481=CYLINDRICAL_SURFACE('',#8442,0.013);
#7482=CYLINDRICAL_SURFACE('',#8446,0.013);
#7483=CYLINDRICAL_SURFACE('',#8450,0.013);
#7484=CYLINDRICAL_SURFACE('',#8454,0.013);
#7485=CYLINDRICAL_SURFACE('',#8458,0.013);
#7486=CYLINDRICAL_SURFACE('',#8462,0.013);
#7487=CYLINDRICAL_SURFACE('',#8466,0.013);
#7488=CYLINDRICAL_SURFACE('',#8470,0.013);
#7489=CYLINDRICAL_SURFACE('',#8474,0.013);
#7490=CYLINDRICAL_SURFACE('',#8478,0.013);
#7491=CYLINDRICAL_SURFACE('',#8482,0.013);
#7492=CYLINDRICAL_SURFACE('',#8486,0.013);
#7493=CYLINDRICAL_SURFACE('',#8490,0.013);
#7494=CYLINDRICAL_SURFACE('',#8494,0.013);
#7495=CYLINDRICAL_SURFACE('',#8498,0.013);
#7496=CYLINDRICAL_SURFACE('',#8502,0.013);
#7497=CYLINDRICAL_SURFACE('',#8506,0.013);
#7498=CYLINDRICAL_SURFACE('',#8510,0.013);
#7499=CYLINDRICAL_SURFACE('',#8514,0.0175);
#7500=CYLINDRICAL_SURFACE('',#8540,0.0165);
#7501=CYLINDRICAL_SURFACE('',#8542,0.0075);
#7502=CYLINDRICAL_SURFACE('',#8553,0.0085);
#7503=CYLINDRICAL_SURFACE('',#8559,0.008);
#7504=CYLINDRICAL_SURFACE('',#8566,0.009);
#7505=CYLINDRICAL_SURFACE('',#8576,0.0085);
#7506=CYLINDRICAL_SURFACE('',#8578,0.0075);
#7507=CYLINDRICAL_SURFACE('',#8589,0.0085);
#7508=CYLINDRICAL_SURFACE('',#8595,0.008);
#7509=CYLINDRICAL_SURFACE('',#8602,0.009);
#7510=CYLINDRICAL_SURFACE('',#8612,0.0085);
#7511=CYLINDRICAL_SURFACE('',#8619,0.012);
#7512=CYLINDRICAL_SURFACE('',#8621,0.01065);
#7513=CYLINDRICAL_SURFACE('',#8630,0.008425);
#7514=CYLINDRICAL_SURFACE('',#8632,0.011075);
#7515=CYLINDRICAL_SURFACE('',#8643,0.00885);
#7516=CYLINDRICAL_SURFACE('',#8645,0.0075);
#7517=CYLINDRICAL_SURFACE('',#8658,0.012);
#7518=CYLINDRICAL_SURFACE('',#8660,0.01065);
#7519=CYLINDRICAL_SURFACE('',#8669,0.008425);
#7520=CYLINDRICAL_SURFACE('',#8671,0.011075);
#7521=CYLINDRICAL_SURFACE('',#8682,0.00885);
#7522=CYLINDRICAL_SURFACE('',#8684,0.0075);
#7523=CYLINDRICAL_SURFACE('',#8692,0.016);
#7524=CYLINDRICAL_SURFACE('',#8699,0.01635);
#7525=CYLINDRICAL_SURFACE('',#8701,0.01635);
#7526=CYLINDRICAL_SURFACE('',#8707,0.016);
#7527=CYLINDRICAL_SURFACE('',#8709,0.016);
#7528=CYLINDRICAL_SURFACE('',#8715,0.01635);
#7529=CYLINDRICAL_SURFACE('',#8717,0.01635);
#7530=CYLINDRICAL_SURFACE('',#8723,0.016);
#7531=CYLINDRICAL_SURFACE('',#8725,0.016);
#7532=CYLINDRICAL_SURFACE('',#8731,0.01635);
#7533=CYLINDRICAL_SURFACE('',#8733,0.01635);
#7534=CYLINDRICAL_SURFACE('',#8739,0.016);
#7535=CYLINDRICAL_SURFACE('',#8741,0.016);
#7536=CYLINDRICAL_SURFACE('',#8747,0.0175);
#7537=CYLINDRICAL_SURFACE('',#8749,0.0125);
#7538=CYLINDRICAL_SURFACE('',#8755,0.0185);
#7539=CYLINDRICAL_SURFACE('',#8757,0.0115);
#7540=CYLINDRICAL_SURFACE('',#8781,0.0013);
#7541=CYLINDRICAL_SURFACE('',#8783,0.0013);
#7542=CYLINDRICAL_SURFACE('',#8785,0.0013);
#7543=CYLINDRICAL_SURFACE('',#8787,0.0013);
#7544=CYLINDRICAL_SURFACE('',#8789,0.0013);
#7545=CYLINDRICAL_SURFACE('',#8791,0.0013);
#7546=CYLINDRICAL_SURFACE('',#8793,0.0013);
#7547=CYLINDRICAL_SURFACE('',#8795,0.0013);
#7548=CYLINDRICAL_SURFACE('',#8797,0.0013);
#7549=CYLINDRICAL_SURFACE('',#8799,0.0013);
#7550=CYLINDRICAL_SURFACE('',#8801,0.0013);
#7551=CYLINDRICAL_SURFACE('',#8803,0.0013);
#7552=CYLINDRICAL_SURFACE('',#8805,0.0013);
#7553=CYLINDRICAL_SURFACE('',#8807,0.0013);
#7554=CYLINDRICAL_SURFACE('',#8809,0.0013);
#7555=CYLINDRICAL_SURFACE('',#8811,0.0013);
#7556=CYLINDRICAL_SURFACE('',#8813,0.0013);
#7557=CYLINDRICAL_SURFACE('',#8815,0.0013);
#7558=CYLINDRICAL_SURFACE('',#8819,0.012);
#7559=CYLINDRICAL_SURFACE('',#8824,0.034);
#7560=CYLINDRICAL_SURFACE('',#8828,0.0195);
#7561=CYLINDRICAL_SURFACE('',#8830,0.0115);
#7562=CYLINDRICAL_SURFACE('',#8839,0.0125);
#7563=CYLINDRICAL_SURFACE('',#8841,0.016035898385);
#7564=CYLINDRICAL_SURFACE('',#8848,0.00149895940068901);
#7565=CYLINDRICAL_SURFACE('',#8851,0.001498959108051);
#7566=CYLINDRICAL_SURFACE('',#8853,0.0014989594008755);
#7567=CYLINDRICAL_SURFACE('',#8856,0.00149895910812507);
#7568=CYLINDRICAL_SURFACE('',#8858,0.00149895940094096);
#7569=CYLINDRICAL_SURFACE('',#8861,0.00149895910814045);
#7570=CYLINDRICAL_SURFACE('',#8865,0.0014989594007659);
#7571=CYLINDRICAL_SURFACE('',#8868,0.00149895910811289);
#7572=CYLINDRICAL_SURFACE('',#8870,0.00149895940089024);
#7573=CYLINDRICAL_SURFACE('',#8873,0.00149895910812507);
#7574=CYLINDRICAL_SURFACE('',#8875,0.00149895940094097);
#7575=CYLINDRICAL_SURFACE('',#8878,0.00149895910814057);
#7576=CYLINDRICAL_SURFACE('',#8881,0.017035898385);
#7577=CYLINDRICAL_SURFACE('',#8883,0.0015);
#7578=CYLINDRICAL_SURFACE('',#8935,0.0015);
#7579=CYLINDRICAL_SURFACE('',#8937,0.017035898385);
#7580=CYLINDRICAL_SURFACE('',#8939,0.0015);
#7581=CYLINDRICAL_SURFACE('',#8941,0.0015);
#7582=CYLINDRICAL_SURFACE('',#8943,0.017035898385);
#7583=CYLINDRICAL_SURFACE('',#8945,0.0015);
#7584=CYLINDRICAL_SURFACE('',#8947,0.0015);
#7585=CYLINDRICAL_SURFACE('',#8949,0.017035898385);
#7586=CYLINDRICAL_SURFACE('',#8951,0.0015);
#7587=CYLINDRICAL_SURFACE('',#8953,0.0015);
#7588=CYLINDRICAL_SURFACE('',#8955,0.017035898385);
#7589=CYLINDRICAL_SURFACE('',#8957,0.0015);
#7590=CYLINDRICAL_SURFACE('',#8959,0.0015);
#7591=CYLINDRICAL_SURFACE('',#8961,0.017035898385);
#7592=CYLINDRICAL_SURFACE('',#8963,0.0015);
#7593=CYLINDRICAL_SURFACE('',#8965,0.0015);
#7594=CYLINDRICAL_SURFACE('',#9009,0.0013);
#7595=CYLINDRICAL_SURFACE('',#9010,0.0013);
#7596=CYLINDRICAL_SURFACE('',#9011,0.0013);
#7597=CYLINDRICAL_SURFACE('',#9012,0.0013);
#7598=CYLINDRICAL_SURFACE('',#9013,0.0013);
#7599=CYLINDRICAL_SURFACE('',#9014,0.0013);
#7600=CYLINDRICAL_SURFACE('',#9015,0.0013);
#7601=CYLINDRICAL_SURFACE('',#9016,0.0013);
#7602=CYLINDRICAL_SURFACE('',#9017,0.0013);
#7603=CYLINDRICAL_SURFACE('',#9018,0.0013);
#7604=CYLINDRICAL_SURFACE('',#9019,0.0013);
#7605=CYLINDRICAL_SURFACE('',#9020,0.0013);
#7606=CYLINDRICAL_SURFACE('',#9021,0.0013);
#7607=CYLINDRICAL_SURFACE('',#9022,0.0013);
#7608=CYLINDRICAL_SURFACE('',#9023,0.0013);
#7609=CYLINDRICAL_SURFACE('',#9024,0.0013);
#7610=CYLINDRICAL_SURFACE('',#9025,0.0013);
#7611=CYLINDRICAL_SURFACE('',#9026,0.0013);
#7612=CYLINDRICAL_SURFACE('',#9028,0.0015);
#7613=CYLINDRICAL_SURFACE('',#9029,0.024);
#7614=CYLINDRICAL_SURFACE('',#9030,0.0015);
#7615=CYLINDRICAL_SURFACE('',#9033,0.0015);
#7616=CYLINDRICAL_SURFACE('',#9034,0.024);
#7617=CYLINDRICAL_SURFACE('',#9035,0.0015);
#7618=CYLINDRICAL_SURFACE('',#9037,0.0015);
#7619=CYLINDRICAL_SURFACE('',#9038,0.024);
#7620=CYLINDRICAL_SURFACE('',#9039,0.0015);
#7621=CYLINDRICAL_SURFACE('',#9042,0.0015);
#7622=CYLINDRICAL_SURFACE('',#9043,0.024);
#7623=CYLINDRICAL_SURFACE('',#9044,0.0015);
#7624=CYLINDRICAL_SURFACE('',#9047,0.0015);
#7625=CYLINDRICAL_SURFACE('',#9048,0.024);
#7626=CYLINDRICAL_SURFACE('',#9049,0.0015);
#7627=CYLINDRICAL_SURFACE('',#9052,0.0015);
#7628=CYLINDRICAL_SURFACE('',#9053,0.024);
#7629=CYLINDRICAL_SURFACE('',#9054,0.0015);
#7630=CYLINDRICAL_SURFACE('',#9058,0.016035898385);
#7631=CYLINDRICAL_SURFACE('',#9064,0.034);
#7632=CYLINDRICAL_SURFACE('',#9067,0.016035898385);
#7633=CYLINDRICAL_SURFACE('',#9115,0.016535898385);
#7634=CYLINDRICAL_SURFACE('',#9119,0.016535898385);
#7635=CYLINDRICAL_SURFACE('',#9120,0.000299999999290666);
#7636=CYLINDRICAL_SURFACE('',#9126,0.016535898385);
#7637=CYLINDRICAL_SURFACE('',#9130,0.016535898385);
#7638=CYLINDRICAL_SURFACE('',#9134,0.016535898385);
#7639=CYLINDRICAL_SURFACE('',#9138,0.016535898385);
#7640=CYLINDRICAL_SURFACE('',#9147,0.00214999999988175);
#7641=CYLINDRICAL_SURFACE('',#9148,0.00215);
#7642=CYLINDRICAL_SURFACE('',#9149,0.00214999999988175);
#7643=CYLINDRICAL_SURFACE('',#9150,0.00214999999988175);
#7644=CYLINDRICAL_SURFACE('',#9151,0.00215);
#7645=CYLINDRICAL_SURFACE('',#9152,0.00214999999988175);
#7646=CYLINDRICAL_SURFACE('',#9153,0.0003);
#7647=CYLINDRICAL_SURFACE('',#9154,0.0003);
#7648=CYLINDRICAL_SURFACE('',#9155,0.024);
#7649=CYLINDRICAL_SURFACE('',#9156,0.0003);
#7650=CYLINDRICAL_SURFACE('',#9157,0.0003);
#7651=CYLINDRICAL_SURFACE('',#9158,0.024);
#7652=CYLINDRICAL_SURFACE('',#9160,0.0003);
#7653=CYLINDRICAL_SURFACE('',#9161,0.024);
#7654=CYLINDRICAL_SURFACE('',#9163,0.0003);
#7655=CYLINDRICAL_SURFACE('',#9164,0.0003);
#7656=CYLINDRICAL_SURFACE('',#9165,0.024);
#7657=CYLINDRICAL_SURFACE('',#9166,0.0003);
#7658=CYLINDRICAL_SURFACE('',#9167,0.0003);
#7659=CYLINDRICAL_SURFACE('',#9168,0.024);
#7660=CYLINDRICAL_SURFACE('',#9169,0.0003);
#7661=CYLINDRICAL_SURFACE('',#9170,0.0003);
#7662=CYLINDRICAL_SURFACE('',#9171,0.024);
#7663=CYLINDRICAL_SURFACE('',#9178,0.0003);
#7664=ADVANCED_FACE('',(#6714,#6715),#7475,.F.);
#7665=ADVANCED_FACE('',(#6716,#6717),#888,.F.);
#7666=ADVANCED_FACE('',(#6718,#6719),#889,.F.);
#7667=ADVANCED_FACE('',(#6720,#6721),#7476,.T.);
#7668=ADVANCED_FACE('',(#6722,#6723),#7477,.T.);
#7669=ADVANCED_FACE('',(#6724),#890,.T.);
#7670=ADVANCED_FACE('',(#6725),#891,.T.);
#7671=ADVANCED_FACE('',(#6726),#892,.F.);
#7672=ADVANCED_FACE('',(#6727),#893,.T.);
#7673=ADVANCED_FACE('',(#6728),#894,.T.);
#7674=ADVANCED_FACE('',(#6729),#895,.T.);
#7675=ADVANCED_FACE('',(#6730),#896,.F.);
#7676=ADVANCED_FACE('',(#6731),#897,.T.);
#7677=ADVANCED_FACE('',(#6732),#898,.T.);
#7678=ADVANCED_FACE('',(#6733),#899,.T.);
#7679=ADVANCED_FACE('',(#6734),#900,.F.);
#7680=ADVANCED_FACE('',(#6735),#901,.T.);
#7681=ADVANCED_FACE('',(#6736),#902,.T.);
#7682=ADVANCED_FACE('',(#6737),#903,.T.);
#7683=ADVANCED_FACE('',(#6738),#904,.F.);
#7684=ADVANCED_FACE('',(#6739),#905,.T.);
#7685=ADVANCED_FACE('',(#6740),#906,.T.);
#7686=ADVANCED_FACE('',(#6741),#907,.T.);
#7687=ADVANCED_FACE('',(#6742),#908,.F.);
#7688=ADVANCED_FACE('',(#6743),#909,.T.);
#7689=ADVANCED_FACE('',(#6744),#910,.T.);
#7690=ADVANCED_FACE('',(#6745),#911,.T.);
#7691=ADVANCED_FACE('',(#6746),#912,.F.);
#7692=ADVANCED_FACE('',(#6747),#913,.T.);
#7693=ADVANCED_FACE('',(#6748),#914,.T.);
#7694=ADVANCED_FACE('',(#6749),#915,.T.);
#7695=ADVANCED_FACE('',(#6750),#916,.F.);
#7696=ADVANCED_FACE('',(#6751),#917,.T.);
#7697=ADVANCED_FACE('',(#6752),#918,.T.);
#7698=ADVANCED_FACE('',(#6753),#919,.T.);
#7699=ADVANCED_FACE('',(#6754),#920,.F.);
#7700=ADVANCED_FACE('',(#6755),#921,.T.);
#7701=ADVANCED_FACE('',(#6756),#922,.T.);
#7702=ADVANCED_FACE('',(#6757),#923,.T.);
#7703=ADVANCED_FACE('',(#6758),#924,.F.);
#7704=ADVANCED_FACE('',(#6759),#925,.T.);
#7705=ADVANCED_FACE('',(#6760),#926,.T.);
#7706=ADVANCED_FACE('',(#6761),#927,.T.);
#7707=ADVANCED_FACE('',(#6762),#928,.F.);
#7708=ADVANCED_FACE('',(#6763),#929,.T.);
#7709=ADVANCED_FACE('',(#6764),#930,.T.);
#7710=ADVANCED_FACE('',(#6765),#931,.T.);
#7711=ADVANCED_FACE('',(#6766),#932,.F.);
#7712=ADVANCED_FACE('',(#6767),#933,.T.);
#7713=ADVANCED_FACE('',(#6768),#934,.T.);
#7714=ADVANCED_FACE('',(#6769),#935,.T.);
#7715=ADVANCED_FACE('',(#6770),#936,.F.);
#7716=ADVANCED_FACE('',(#6771),#937,.T.);
#7717=ADVANCED_FACE('',(#6772),#938,.T.);
#7718=ADVANCED_FACE('',(#6773),#939,.T.);
#7719=ADVANCED_FACE('',(#6774),#940,.F.);
#7720=ADVANCED_FACE('',(#6775),#941,.T.);
#7721=ADVANCED_FACE('',(#6776),#942,.T.);
#7722=ADVANCED_FACE('',(#6777),#943,.T.);
#7723=ADVANCED_FACE('',(#6778),#944,.F.);
#7724=ADVANCED_FACE('',(#6779),#945,.T.);
#7725=ADVANCED_FACE('',(#6780),#946,.T.);
#7726=ADVANCED_FACE('',(#6781),#947,.T.);
#7727=ADVANCED_FACE('',(#6782),#948,.F.);
#7728=ADVANCED_FACE('',(#6783),#949,.T.);
#7729=ADVANCED_FACE('',(#6784),#950,.T.);
#7730=ADVANCED_FACE('',(#6785),#951,.T.);
#7731=ADVANCED_FACE('',(#6786),#952,.F.);
#7732=ADVANCED_FACE('',(#6787),#953,.T.);
#7733=ADVANCED_FACE('',(#6788),#954,.T.);
#7734=ADVANCED_FACE('',(#6789),#955,.T.);
#7735=ADVANCED_FACE('',(#6790),#956,.F.);
#7736=ADVANCED_FACE('',(#6791),#957,.T.);
#7737=ADVANCED_FACE('',(#6792),#958,.T.);
#7738=ADVANCED_FACE('',(#6793),#959,.T.);
#7739=ADVANCED_FACE('',(#6794),#960,.F.);
#7740=ADVANCED_FACE('',(#6795),#961,.T.);
#7741=ADVANCED_FACE('',(#6796),#962,.T.);
#7742=ADVANCED_FACE('',(#6797),#963,.T.);
#7743=ADVANCED_FACE('',(#6798),#964,.F.);
#7744=ADVANCED_FACE('',(#6799),#965,.T.);
#7745=ADVANCED_FACE('',(#6800),#966,.T.);
#7746=ADVANCED_FACE('',(#6801),#967,.T.);
#7747=ADVANCED_FACE('',(#6802),#968,.F.);
#7748=ADVANCED_FACE('',(#6803),#969,.T.);
#7749=ADVANCED_FACE('',(#6804,#6805),#970,.F.);
#7750=ADVANCED_FACE('',(#6806),#7478,.T.);
#7751=ADVANCED_FACE('',(#6807),#971,.F.);
#7752=ADVANCED_FACE('',(#6808),#972,.F.);
#7753=ADVANCED_FACE('',(#6809,#6810),#7479,.T.);
#7754=ADVANCED_FACE('',(#6811),#7480,.T.);
#7755=ADVANCED_FACE('',(#6812),#973,.F.);
#7756=ADVANCED_FACE('',(#6813),#974,.F.);
#7757=ADVANCED_FACE('',(#6814),#7481,.T.);
#7758=ADVANCED_FACE('',(#6815),#975,.F.);
#7759=ADVANCED_FACE('',(#6816),#976,.F.);
#7760=ADVANCED_FACE('',(#6817),#7482,.T.);
#7761=ADVANCED_FACE('',(#6818),#977,.F.);
#7762=ADVANCED_FACE('',(#6819),#978,.F.);
#7763=ADVANCED_FACE('',(#6820),#7483,.T.);
#7764=ADVANCED_FACE('',(#6821),#979,.F.);
#7765=ADVANCED_FACE('',(#6822),#980,.F.);
#7766=ADVANCED_FACE('',(#6823),#7484,.T.);
#7767=ADVANCED_FACE('',(#6824),#981,.F.);
#7768=ADVANCED_FACE('',(#6825),#982,.F.);
#7769=ADVANCED_FACE('',(#6826),#7485,.T.);
#7770=ADVANCED_FACE('',(#6827),#983,.F.);
#7771=ADVANCED_FACE('',(#6828),#984,.F.);
#7772=ADVANCED_FACE('',(#6829),#7486,.T.);
#7773=ADVANCED_FACE('',(#6830),#985,.F.);
#7774=ADVANCED_FACE('',(#6831),#986,.F.);
#7775=ADVANCED_FACE('',(#6832),#7487,.T.);
#7776=ADVANCED_FACE('',(#6833),#987,.F.);
#7777=ADVANCED_FACE('',(#6834),#988,.F.);
#7778=ADVANCED_FACE('',(#6835),#7488,.T.);
#7779=ADVANCED_FACE('',(#6836),#989,.F.);
#7780=ADVANCED_FACE('',(#6837),#990,.F.);
#7781=ADVANCED_FACE('',(#6838),#7489,.T.);
#7782=ADVANCED_FACE('',(#6839),#991,.F.);
#7783=ADVANCED_FACE('',(#6840),#992,.F.);
#7784=ADVANCED_FACE('',(#6841),#7490,.T.);
#7785=ADVANCED_FACE('',(#6842),#993,.F.);
#7786=ADVANCED_FACE('',(#6843),#994,.F.);
#7787=ADVANCED_FACE('',(#6844),#7491,.T.);
#7788=ADVANCED_FACE('',(#6845),#995,.F.);
#7789=ADVANCED_FACE('',(#6846),#996,.F.);
#7790=ADVANCED_FACE('',(#6847),#7492,.T.);
#7791=ADVANCED_FACE('',(#6848),#997,.F.);
#7792=ADVANCED_FACE('',(#6849),#998,.F.);
#7793=ADVANCED_FACE('',(#6850),#7493,.T.);
#7794=ADVANCED_FACE('',(#6851),#999,.F.);
#7795=ADVANCED_FACE('',(#6852),#1000,.F.);
#7796=ADVANCED_FACE('',(#6853),#7494,.T.);
#7797=ADVANCED_FACE('',(#6854),#1001,.F.);
#7798=ADVANCED_FACE('',(#6855),#1002,.F.);
#7799=ADVANCED_FACE('',(#6856),#7495,.T.);
#7800=ADVANCED_FACE('',(#6857),#1003,.F.);
#7801=ADVANCED_FACE('',(#6858),#1004,.F.);
#7802=ADVANCED_FACE('',(#6859),#7496,.T.);
#7803=ADVANCED_FACE('',(#6860),#1005,.F.);
#7804=ADVANCED_FACE('',(#6861),#1006,.F.);
#7805=ADVANCED_FACE('',(#6862),#7497,.T.);
#7806=ADVANCED_FACE('',(#6863),#1007,.F.);
#7807=ADVANCED_FACE('',(#6864),#1008,.F.);
#7808=ADVANCED_FACE('',(#6865),#7498,.T.);
#7809=ADVANCED_FACE('',(#6866),#1009,.F.);
#7810=ADVANCED_FACE('',(#6867),#1010,.F.);
#7811=ADVANCED_FACE('',(#6868,#6869),#7499,.T.);
#7812=ADVANCED_FACE('',(#6870),#1011,.T.);
#7813=ADVANCED_FACE('',(#6871),#1012,.T.);
#7814=ADVANCED_FACE('',(#6872,#6873),#1013,.F.);
#7815=ADVANCED_FACE('',(#6874),#1014,.T.);
#7816=ADVANCED_FACE('',(#6875),#1015,.T.);
#7817=ADVANCED_FACE('',(#6876),#1016,.T.);
#7818=ADVANCED_FACE('',(#6877),#1017,.T.);
#7819=ADVANCED_FACE('',(#6878),#1018,.T.);
#7820=ADVANCED_FACE('',(#6879),#1019,.T.);
#7821=ADVANCED_FACE('',(#6880),#1020,.T.);
#7822=ADVANCED_FACE('',(#6881),#1021,.T.);
#7823=ADVANCED_FACE('',(#6882),#1022,.T.);
#7824=ADVANCED_FACE('',(#6883),#1023,.T.);
#7825=ADVANCED_FACE('',(#6884),#1024,.T.);
#7826=ADVANCED_FACE('',(#6885),#1025,.T.);
#7827=ADVANCED_FACE('',(#6886),#1026,.T.);
#7828=ADVANCED_FACE('',(#6887),#1027,.T.);
#7829=ADVANCED_FACE('',(#6888),#1028,.T.);
#7830=ADVANCED_FACE('',(#6889),#1029,.T.);
#7831=ADVANCED_FACE('',(#6890),#1030,.T.);
#7832=ADVANCED_FACE('',(#6891),#1031,.T.);
#7833=ADVANCED_FACE('',(#6892,#6893),#1032,.F.);
#7834=ADVANCED_FACE('',(#6894,#6895),#7500,.T.);
#7835=ADVANCED_FACE('',(#6896,#6897),#7501,.F.);
#7836=ADVANCED_FACE('',(#6898,#6899),#1033,.F.);
#7837=ADVANCED_FACE('',(#6900,#6901),#1034,.F.);
#7838=ADVANCED_FACE('',(#6902,#6903),#34,.T.);
#7839=ADVANCED_FACE('',(#6904,#6905),#35,.T.);
#7840=ADVANCED_FACE('',(#6906,#6907),#7502,.T.);
#7841=ADVANCED_FACE('',(#6908,#6909),#36,.T.);
#7842=ADVANCED_FACE('',(#6910,#6911),#1035,.F.);
#7843=ADVANCED_FACE('',(#6912,#6913),#7503,.T.);
#7844=ADVANCED_FACE('',(#6914,#6915),#37,.F.);
#7845=ADVANCED_FACE('',(#6916),#38,.F.);
#7846=ADVANCED_FACE('',(#6917),#39,.F.);
#7847=ADVANCED_FACE('',(#6918,#6919),#7504,.T.);
#7848=ADVANCED_FACE('',(#6920,#6921),#23,.T.);
#7849=ADVANCED_FACE('',(#6922),#40,.T.);
#7850=ADVANCED_FACE('',(#6923),#41,.T.);
#7851=ADVANCED_FACE('',(#6924),#42,.T.);
#7852=ADVANCED_FACE('',(#6925),#43,.T.);
#7853=ADVANCED_FACE('',(#6926,#6927),#7505,.T.);
#7854=ADVANCED_FACE('',(#6928,#6929),#7506,.F.);
#7855=ADVANCED_FACE('',(#6930,#6931),#1036,.F.);
#7856=ADVANCED_FACE('',(#6932,#6933),#1037,.F.);
#7857=ADVANCED_FACE('',(#6934,#6935),#44,.T.);
#7858=ADVANCED_FACE('',(#6936,#6937),#45,.T.);
#7859=ADVANCED_FACE('',(#6938,#6939),#7507,.T.);
#7860=ADVANCED_FACE('',(#6940,#6941),#46,.T.);
#7861=ADVANCED_FACE('',(#6942,#6943),#1038,.F.);
#7862=ADVANCED_FACE('',(#6944,#6945),#7508,.T.);
#7863=ADVANCED_FACE('',(#6946,#6947),#47,.F.);
#7864=ADVANCED_FACE('',(#6948),#48,.F.);
#7865=ADVANCED_FACE('',(#6949),#49,.F.);
#7866=ADVANCED_FACE('',(#6950,#6951),#7509,.T.);
#7867=ADVANCED_FACE('',(#6952,#6953),#24,.T.);
#7868=ADVANCED_FACE('',(#6954),#50,.T.);
#7869=ADVANCED_FACE('',(#6955),#51,.T.);
#7870=ADVANCED_FACE('',(#6956),#52,.T.);
#7871=ADVANCED_FACE('',(#6957),#53,.T.);
#7872=ADVANCED_FACE('',(#6958,#6959),#7510,.T.);
#7873=ADVANCED_FACE('',(#6960,#6961),#54,.T.);
#7874=ADVANCED_FACE('',(#6962,#6963),#1039,.T.);
#7875=ADVANCED_FACE('',(#6964,#6965),#7511,.T.);
#7876=ADVANCED_FACE('',(#6966,#6967),#7512,.F.);
#7877=ADVANCED_FACE('',(#6968,#6969),#55,.T.);
#7878=ADVANCED_FACE('',(#6970),#56,.T.);
#7879=ADVANCED_FACE('',(#6971),#57,.T.);
#7880=ADVANCED_FACE('',(#6972,#6973),#1040,.T.);
#7881=ADVANCED_FACE('',(#6974,#6975),#7513,.T.);
#7882=ADVANCED_FACE('',(#6976,#6977),#7514,.F.);
#7883=ADVANCED_FACE('',(#6978,#6979),#1041,.T.);
#7884=ADVANCED_FACE('',(#6980),#58,.T.);
#7885=ADVANCED_FACE('',(#6981),#59,.T.);
#7886=ADVANCED_FACE('',(#6982),#60,.T.);
#7887=ADVANCED_FACE('',(#6983),#61,.T.);
#7888=ADVANCED_FACE('',(#6984,#6985),#7515,.T.);
#7889=ADVANCED_FACE('',(#6986,#6987),#7516,.F.);
#7890=ADVANCED_FACE('',(#6988,#6989),#1042,.T.);
#7891=ADVANCED_FACE('',(#6990),#62,.T.);
#7892=ADVANCED_FACE('',(#6991),#63,.T.);
#7893=ADVANCED_FACE('',(#6992,#6993),#64,.T.);
#7894=ADVANCED_FACE('',(#6994,#6995),#1043,.T.);
#7895=ADVANCED_FACE('',(#6996,#6997),#7517,.T.);
#7896=ADVANCED_FACE('',(#6998,#6999),#7518,.F.);
#7897=ADVANCED_FACE('',(#7000,#7001),#65,.T.);
#7898=ADVANCED_FACE('',(#7002),#66,.T.);
#7899=ADVANCED_FACE('',(#7003),#67,.T.);
#7900=ADVANCED_FACE('',(#7004,#7005),#1044,.T.);
#7901=ADVANCED_FACE('',(#7006,#7007),#7519,.T.);
#7902=ADVANCED_FACE('',(#7008,#7009),#7520,.F.);
#7903=ADVANCED_FACE('',(#7010,#7011),#1045,.T.);
#7904=ADVANCED_FACE('',(#7012),#68,.T.);
#7905=ADVANCED_FACE('',(#7013),#69,.T.);
#7906=ADVANCED_FACE('',(#7014),#70,.T.);
#7907=ADVANCED_FACE('',(#7015),#71,.T.);
#7908=ADVANCED_FACE('',(#7016,#7017),#7521,.T.);
#7909=ADVANCED_FACE('',(#7018,#7019),#7522,.F.);
#7910=ADVANCED_FACE('',(#7020,#7021),#1046,.T.);
#7911=ADVANCED_FACE('',(#7022),#72,.T.);
#7912=ADVANCED_FACE('',(#7023),#73,.T.);
#7913=ADVANCED_FACE('',(#7024,#7025),#7523,.F.);
#7914=ADVANCED_FACE('',(#7026,#7027),#1047,.T.);
#7915=ADVANCED_FACE('',(#7028,#7029),#1048,.T.);
#7916=ADVANCED_FACE('',(#7030,#7031),#7524,.F.);
#7917=ADVANCED_FACE('',(#7032,#7033),#7525,.F.);
#7918=ADVANCED_FACE('',(#7034,#7035),#1049,.T.);
#7919=ADVANCED_FACE('',(#7036,#7037),#1050,.T.);
#7920=ADVANCED_FACE('',(#7038,#7039),#7526,.F.);
#7921=ADVANCED_FACE('',(#7040,#7041),#7527,.F.);
#7922=ADVANCED_FACE('',(#7042,#7043),#1051,.T.);
#7923=ADVANCED_FACE('',(#7044,#7045),#1052,.T.);
#7924=ADVANCED_FACE('',(#7046,#7047),#7528,.F.);
#7925=ADVANCED_FACE('',(#7048,#7049),#7529,.F.);
#7926=ADVANCED_FACE('',(#7050,#7051),#1053,.T.);
#7927=ADVANCED_FACE('',(#7052,#7053),#1054,.T.);
#7928=ADVANCED_FACE('',(#7054,#7055),#7530,.F.);
#7929=ADVANCED_FACE('',(#7056,#7057),#7531,.F.);
#7930=ADVANCED_FACE('',(#7058,#7059),#1055,.T.);
#7931=ADVANCED_FACE('',(#7060,#7061),#1056,.T.);
#7932=ADVANCED_FACE('',(#7062,#7063),#7532,.F.);
#7933=ADVANCED_FACE('',(#7064,#7065),#7533,.F.);
#7934=ADVANCED_FACE('',(#7066,#7067),#1057,.T.);
#7935=ADVANCED_FACE('',(#7068,#7069),#1058,.T.);
#7936=ADVANCED_FACE('',(#7070,#7071),#7534,.F.);
#7937=ADVANCED_FACE('',(#7072,#7073),#7535,.F.);
#7938=ADVANCED_FACE('',(#7074,#7075),#1059,.T.);
#7939=ADVANCED_FACE('',(#7076,#7077),#1060,.T.);
#7940=ADVANCED_FACE('',(#7078,#7079),#7536,.F.);
#7941=ADVANCED_FACE('',(#7080,#7081),#7537,.F.);
#7942=ADVANCED_FACE('',(#7082,#7083),#1061,.F.);
#7943=ADVANCED_FACE('',(#7084,#7085),#1062,.T.);
#7944=ADVANCED_FACE('',(#7086,#7087),#7538,.T.);
#7945=ADVANCED_FACE('',(#7088,#7089),#7539,.F.);
#7946=ADVANCED_FACE('',(#7090,#7091,#7092,#7093,#7094,#7095,#7096,#7097,
#7098,#7099,#7100,#7101,#7102,#7103,#7104,#7105,#7106,#7107,#7108,#7109),
#1063,.F.);
#7947=ADVANCED_FACE('',(#7110,#7111),#25,.F.);
#7948=ADVANCED_FACE('',(#7112,#7113),#7540,.F.);
#7949=ADVANCED_FACE('',(#7114,#7115),#7541,.F.);
#7950=ADVANCED_FACE('',(#7116,#7117),#7542,.F.);
#7951=ADVANCED_FACE('',(#7118,#7119),#7543,.F.);
#7952=ADVANCED_FACE('',(#7120,#7121),#7544,.F.);
#7953=ADVANCED_FACE('',(#7122,#7123),#7545,.F.);
#7954=ADVANCED_FACE('',(#7124,#7125),#7546,.F.);
#7955=ADVANCED_FACE('',(#7126,#7127),#7547,.F.);
#7956=ADVANCED_FACE('',(#7128,#7129),#7548,.F.);
#7957=ADVANCED_FACE('',(#7130,#7131),#7549,.F.);
#7958=ADVANCED_FACE('',(#7132,#7133),#7550,.F.);
#7959=ADVANCED_FACE('',(#7134,#7135),#7551,.F.);
#7960=ADVANCED_FACE('',(#7136,#7137),#7552,.F.);
#7961=ADVANCED_FACE('',(#7138,#7139),#7553,.F.);
#7962=ADVANCED_FACE('',(#7140,#7141),#7554,.F.);
#7963=ADVANCED_FACE('',(#7142,#7143),#7555,.F.);
#7964=ADVANCED_FACE('',(#7144,#7145),#7556,.F.);
#7965=ADVANCED_FACE('',(#7146,#7147),#7557,.F.);
#7966=ADVANCED_FACE('',(#7148,#7149),#74,.T.);
#7967=ADVANCED_FACE('',(#7150,#7151),#7558,.F.);
#7968=ADVANCED_FACE('',(#7152,#7153,#7154,#7155,#7156,#7157,#7158,#7159,
#7160,#7161,#7162,#7163,#7164,#7165,#7166,#7167,#7168,#7169,#7170,#7171),
#1064,.F.);
#7969=ADVANCED_FACE('',(#7172,#7173),#7559,.T.);
#7970=ADVANCED_FACE('',(#7174,#7175),#26,.F.);
#7971=ADVANCED_FACE('',(#7176,#7177),#7560,.T.);
#7972=ADVANCED_FACE('',(#7178,#7179),#75,.T.);
#7973=ADVANCED_FACE('',(#7180,#7181),#7561,.F.);
#7974=ADVANCED_FACE('',(#7182,#7183),#27,.T.);
#7975=ADVANCED_FACE('',(#7184,#7185),#1065,.T.);
#7976=ADVANCED_FACE('',(#7186),#76,.F.);
#7977=ADVANCED_FACE('',(#7187),#77,.F.);
#7978=ADVANCED_FACE('',(#7188,#7189),#7562,.F.);
#7979=ADVANCED_FACE('',(#7190,#7191),#7563,.T.);
#7980=ADVANCED_FACE('',(#7192,#7193),#78,.T.);
#7981=ADVANCED_FACE('',(#7194),#79,.F.);
#7982=ADVANCED_FACE('',(#7195),#7564,.F.);
#7983=ADVANCED_FACE('',(#7196),#80,.F.);
#7984=ADVANCED_FACE('',(#7197),#7565,.F.);
#7985=ADVANCED_FACE('',(#7198),#81,.F.);
#7986=ADVANCED_FACE('',(#7199),#7566,.F.);
#7987=ADVANCED_FACE('',(#7200),#82,.F.);
#7988=ADVANCED_FACE('',(#7201),#7567,.F.);
#7989=ADVANCED_FACE('',(#7202),#83,.F.);
#7990=ADVANCED_FACE('',(#7203),#7568,.F.);
#7991=ADVANCED_FACE('',(#7204),#84,.F.);
#7992=ADVANCED_FACE('',(#7205),#7569,.F.);
#7993=ADVANCED_FACE('',(#7206),#85,.F.);
#7994=ADVANCED_FACE('',(#7207),#86,.F.);
#7995=ADVANCED_FACE('',(#7208),#7570,.F.);
#7996=ADVANCED_FACE('',(#7209),#87,.F.);
#7997=ADVANCED_FACE('',(#7210),#7571,.F.);
#7998=ADVANCED_FACE('',(#7211),#88,.F.);
#7999=ADVANCED_FACE('',(#7212),#7572,.F.);
#8000=ADVANCED_FACE('',(#7213),#89,.F.);
#8001=ADVANCED_FACE('',(#7214),#7573,.F.);
#8002=ADVANCED_FACE('',(#7215),#90,.F.);
#8003=ADVANCED_FACE('',(#7216),#7574,.F.);
#8004=ADVANCED_FACE('',(#7217),#91,.F.);
#8005=ADVANCED_FACE('',(#7218),#7575,.F.);
#8006=ADVANCED_FACE('',(#7219,#7220),#1066,.F.);
#8007=ADVANCED_FACE('',(#7221),#7576,.T.);
#8008=ADVANCED_FACE('',(#7222),#7577,.F.);
#8009=ADVANCED_FACE('',(#7223,#7224,#7225,#7226,#7227,#7228,#7229,#7230,
#7231,#7232,#7233,#7234,#7235,#7236,#7237,#7238,#7239,#7240,#7241,#7242),
#1067,.F.);
#8010=ADVANCED_FACE('',(#7243),#7578,.F.);
#8011=ADVANCED_FACE('',(#7244),#7579,.T.);
#8012=ADVANCED_FACE('',(#7245),#7580,.F.);
#8013=ADVANCED_FACE('',(#7246),#7581,.F.);
#8014=ADVANCED_FACE('',(#7247),#7582,.T.);
#8015=ADVANCED_FACE('',(#7248),#7583,.F.);
#8016=ADVANCED_FACE('',(#7249),#7584,.F.);
#8017=ADVANCED_FACE('',(#7250),#7585,.T.);
#8018=ADVANCED_FACE('',(#7251),#7586,.F.);
#8019=ADVANCED_FACE('',(#7252),#7587,.F.);
#8020=ADVANCED_FACE('',(#7253),#7588,.T.);
#8021=ADVANCED_FACE('',(#7254),#7589,.F.);
#8022=ADVANCED_FACE('',(#7255),#7590,.F.);
#8023=ADVANCED_FACE('',(#7256),#7591,.T.);
#8024=ADVANCED_FACE('',(#7257),#7592,.F.);
#8025=ADVANCED_FACE('',(#7258),#7593,.F.);
#8026=ADVANCED_FACE('',(#7259,#7260),#92,.T.);
#8027=ADVANCED_FACE('',(#7261,#7262,#7263,#7264,#7265,#7266,#7267,#7268,
#7269,#7270,#7271,#7272,#7273,#7274,#7275,#7276,#7277,#7278,#7279,#7280,
#7281,#7282,#7283,#7284,#7285,#7286),#1068,.F.);
#8028=ADVANCED_FACE('',(#7287),#1069,.F.);
#8029=ADVANCED_FACE('',(#7288,#7289),#7594,.F.);
#8030=ADVANCED_FACE('',(#7290,#7291),#7595,.F.);
#8031=ADVANCED_FACE('',(#7292,#7293),#7596,.F.);
#8032=ADVANCED_FACE('',(#7294,#7295),#7597,.F.);
#8033=ADVANCED_FACE('',(#7296,#7297),#7598,.F.);
#8034=ADVANCED_FACE('',(#7298,#7299),#7599,.F.);
#8035=ADVANCED_FACE('',(#7300,#7301),#7600,.F.);
#8036=ADVANCED_FACE('',(#7302,#7303),#7601,.F.);
#8037=ADVANCED_FACE('',(#7304,#7305),#7602,.F.);
#8038=ADVANCED_FACE('',(#7306,#7307),#7603,.F.);
#8039=ADVANCED_FACE('',(#7308,#7309),#7604,.F.);
#8040=ADVANCED_FACE('',(#7310,#7311),#7605,.F.);
#8041=ADVANCED_FACE('',(#7312,#7313),#7606,.F.);
#8042=ADVANCED_FACE('',(#7314,#7315),#7607,.F.);
#8043=ADVANCED_FACE('',(#7316,#7317),#7608,.F.);
#8044=ADVANCED_FACE('',(#7318,#7319),#7609,.F.);
#8045=ADVANCED_FACE('',(#7320,#7321),#7610,.F.);
#8046=ADVANCED_FACE('',(#7322,#7323),#7611,.F.);
#8047=ADVANCED_FACE('',(#7324),#1070,.F.);
#8048=ADVANCED_FACE('',(#7325),#7612,.F.);
#8049=ADVANCED_FACE('',(#7326),#7613,.F.);
#8050=ADVANCED_FACE('',(#7327),#7614,.F.);
#8051=ADVANCED_FACE('',(#7328),#1071,.F.);
#8052=ADVANCED_FACE('',(#7329),#1072,.F.);
#8053=ADVANCED_FACE('',(#7330),#7615,.F.);
#8054=ADVANCED_FACE('',(#7331),#7616,.F.);
#8055=ADVANCED_FACE('',(#7332),#7617,.F.);
#8056=ADVANCED_FACE('',(#7333),#1073,.F.);
#8057=ADVANCED_FACE('',(#7334),#7618,.F.);
#8058=ADVANCED_FACE('',(#7335),#7619,.F.);
#8059=ADVANCED_FACE('',(#7336),#7620,.F.);
#8060=ADVANCED_FACE('',(#7337),#1074,.F.);
#8061=ADVANCED_FACE('',(#7338),#1075,.F.);
#8062=ADVANCED_FACE('',(#7339),#7621,.F.);
#8063=ADVANCED_FACE('',(#7340),#7622,.F.);
#8064=ADVANCED_FACE('',(#7341),#7623,.F.);
#8065=ADVANCED_FACE('',(#7342),#1076,.F.);
#8066=ADVANCED_FACE('',(#7343),#1077,.F.);
#8067=ADVANCED_FACE('',(#7344),#7624,.F.);
#8068=ADVANCED_FACE('',(#7345),#7625,.F.);
#8069=ADVANCED_FACE('',(#7346),#7626,.F.);
#8070=ADVANCED_FACE('',(#7347),#1078,.F.);
#8071=ADVANCED_FACE('',(#7348),#1079,.F.);
#8072=ADVANCED_FACE('',(#7349),#7627,.F.);
#8073=ADVANCED_FACE('',(#7350),#7628,.F.);
#8074=ADVANCED_FACE('',(#7351),#7629,.F.);
#8075=ADVANCED_FACE('',(#7352),#1080,.F.);
#8076=ADVANCED_FACE('',(#7353,#7354),#93,.T.);
#8077=ADVANCED_FACE('',(#7355,#7356),#7630,.T.);
#8078=ADVANCED_FACE('',(#7357,#7358),#94,.F.);
#8079=ADVANCED_FACE('',(#7359,#7360),#95,.T.);
#8080=ADVANCED_FACE('',(#7361,#7362),#7631,.T.);
#8081=ADVANCED_FACE('',(#7363,#7364),#96,.F.);
#8082=ADVANCED_FACE('',(#7365,#7366),#7632,.T.);
#8083=ADVANCED_FACE('',(#7367,#7368,#7369,#7370,#7371,#7372,#7373,#7374),
#1081,.F.);
#8084=ADVANCED_FACE('',(#7375),#97,.F.);
#8085=ADVANCED_FACE('',(#7376),#98,.F.);
#8086=ADVANCED_FACE('',(#7377,#7378),#99,.T.);
#8087=ADVANCED_FACE('',(#7379),#100,.T.);
#8088=ADVANCED_FACE('',(#7380),#101,.T.);
#8089=ADVANCED_FACE('',(#7381,#7382),#102,.T.);
#8090=ADVANCED_FACE('',(#7383,#7384),#103,.T.);
#8091=ADVANCED_FACE('',(#7385),#104,.T.);
#8092=ADVANCED_FACE('',(#7386),#105,.T.);
#8093=ADVANCED_FACE('',(#7387,#7388),#106,.T.);
#8094=ADVANCED_FACE('',(#7389),#1082,.F.);
#8095=ADVANCED_FACE('',(#7390),#107,.T.);
#8096=ADVANCED_FACE('',(#7391),#1083,.F.);
#8097=ADVANCED_FACE('',(#7392),#7633,.T.);
#8098=ADVANCED_FACE('',(#7393),#1084,.F.);
#8099=ADVANCED_FACE('',(#7394),#108,.T.);
#8100=ADVANCED_FACE('',(#7395),#1085,.F.);
#8101=ADVANCED_FACE('',(#7396),#7634,.T.);
#8102=ADVANCED_FACE('',(#7397),#7635,.T.);
#8103=ADVANCED_FACE('',(#7398),#109,.T.);
#8104=ADVANCED_FACE('',(#7399),#1086,.F.);
#8105=ADVANCED_FACE('',(#7400),#7636,.T.);
#8106=ADVANCED_FACE('',(#7401),#1087,.F.);
#8107=ADVANCED_FACE('',(#7402),#110,.T.);
#8108=ADVANCED_FACE('',(#7403),#1088,.F.);
#8109=ADVANCED_FACE('',(#7404),#7637,.T.);
#8110=ADVANCED_FACE('',(#7405),#1089,.F.);
#8111=ADVANCED_FACE('',(#7406),#111,.T.);
#8112=ADVANCED_FACE('',(#7407),#1090,.F.);
#8113=ADVANCED_FACE('',(#7408),#7638,.T.);
#8114=ADVANCED_FACE('',(#7409),#1091,.F.);
#8115=ADVANCED_FACE('',(#7410),#112,.T.);
#8116=ADVANCED_FACE('',(#7411),#1092,.F.);
#8117=ADVANCED_FACE('',(#7412),#7639,.T.);
#8118=ADVANCED_FACE('',(#7413,#7414),#28,.T.);
#8119=ADVANCED_FACE('',(#7415,#7416),#29,.T.);
#8120=ADVANCED_FACE('',(#7417),#1093,.F.);
#8121=ADVANCED_FACE('',(#7418,#7419),#30,.T.);
#8122=ADVANCED_FACE('',(#7420,#7421),#31,.T.);
#8123=ADVANCED_FACE('',(#7422,#7423),#32,.T.);
#8124=ADVANCED_FACE('',(#7424,#7425),#33,.T.);
#8125=ADVANCED_FACE('',(#7426,#7427),#7640,.F.);
#8126=ADVANCED_FACE('',(#7428,#7429),#7641,.F.);
#8127=ADVANCED_FACE('',(#7430,#7431),#7642,.F.);
#8128=ADVANCED_FACE('',(#7432,#7433),#7643,.F.);
#8129=ADVANCED_FACE('',(#7434,#7435),#7644,.F.);
#8130=ADVANCED_FACE('',(#7436,#7437),#7645,.F.);
#8131=ADVANCED_FACE('',(#7438),#7646,.T.);
#8132=ADVANCED_FACE('',(#7439),#7647,.T.);
#8133=ADVANCED_FACE('',(#7440),#7648,.T.);
#8134=ADVANCED_FACE('',(#7441),#7649,.T.);
#8135=ADVANCED_FACE('',(#7442),#7650,.T.);
#8136=ADVANCED_FACE('',(#7443),#7651,.T.);
#8137=ADVANCED_FACE('',(#7444),#22,.T.);
#8138=ADVANCED_FACE('',(#7445),#7652,.T.);
#8139=ADVANCED_FACE('',(#7446),#7653,.T.);
#8140=ADVANCED_FACE('',(#7447),#7654,.T.);
#8141=ADVANCED_FACE('',(#7448),#7655,.T.);
#8142=ADVANCED_FACE('',(#7449),#7656,.T.);
#8143=ADVANCED_FACE('',(#7450),#7657,.T.);
#8144=ADVANCED_FACE('',(#7451),#7658,.T.);
#8145=ADVANCED_FACE('',(#7452),#7659,.T.);
#8146=ADVANCED_FACE('',(#7453),#7660,.T.);
#8147=ADVANCED_FACE('',(#7454),#7661,.T.);
#8148=ADVANCED_FACE('',(#7455),#7662,.T.);
#8149=ADVANCED_FACE('',(#7456),#10,.T.);
#8150=ADVANCED_FACE('',(#7457),#11,.T.);
#8151=ADVANCED_FACE('',(#7458),#113,.T.);
#8152=ADVANCED_FACE('',(#7459),#12,.T.);
#8153=ADVANCED_FACE('',(#7460),#13,.T.);
#8154=ADVANCED_FACE('',(#7461),#114,.T.);
#8155=ADVANCED_FACE('',(#7462),#7663,.T.);
#8156=ADVANCED_FACE('',(#7463),#14,.T.);
#8157=ADVANCED_FACE('',(#7464),#15,.T.);
#8158=ADVANCED_FACE('',(#7465),#115,.T.);
#8159=ADVANCED_FACE('',(#7466),#16,.T.);
#8160=ADVANCED_FACE('',(#7467),#17,.T.);
#8161=ADVANCED_FACE('',(#7468),#116,.T.);
#8162=ADVANCED_FACE('',(#7469),#18,.T.);
#8163=ADVANCED_FACE('',(#7470),#19,.T.);
#8164=ADVANCED_FACE('',(#7471),#117,.T.);
#8165=ADVANCED_FACE('',(#7472),#20,.T.);
#8166=ADVANCED_FACE('',(#7473),#21,.T.);
#8167=ADVANCED_FACE('',(#7474),#118,.T.);
#8168=CLOSED_SHELL('',(#7664,#7665,#7666,#7667,#7668,#7669,#7670,#7671,
#7672,#7673,#7674,#7675,#7676,#7677,#7678,#7679,#7680,#7681,#7682,#7683,
#7684,#7685,#7686,#7687,#7688,#7689,#7690,#7691,#7692,#7693,#7694,#7695,
#7696,#7697,#7698,#7699,#7700,#7701,#7702,#7703,#7704,#7705,#7706,#7707,
#7708,#7709,#7710,#7711,#7712,#7713,#7714,#7715,#7716,#7717,#7718,#7719,
#7720,#7721,#7722,#7723,#7724,#7725,#7726,#7727,#7728,#7729,#7730,#7731,
#7732,#7733,#7734,#7735,#7736,#7737,#7738,#7739,#7740,#7741,#7742,#7743,
#7744,#7745,#7746,#7747,#7748,#7749,#7750,#7751,#7752,#7753,#7754,#7755,
#7756,#7757,#7758,#7759,#7760,#7761,#7762,#7763,#7764,#7765,#7766,#7767,
#7768,#7769,#7770,#7771,#7772,#7773,#7774,#7775,#7776,#7777,#7778,#7779,
#7780,#7781,#7782,#7783,#7784,#7785,#7786,#7787,#7788,#7789,#7790,#7791,
#7792,#7793,#7794,#7795,#7796,#7797,#7798,#7799,#7800,#7801,#7802,#7803,
#7804,#7805,#7806,#7807,#7808,#7809,#7810,#7811,#7812,#7813,#7814,#7815,
#7816,#7817,#7818,#7819,#7820,#7821,#7822,#7823,#7824,#7825,#7826,#7827,
#7828,#7829,#7830,#7831,#7832,#7833,#7834));
#8169=CLOSED_SHELL('',(#7835,#7836,#7837,#7838,#7839,#7840,#7841,#7842,
#7843,#7844,#7845,#7846,#7847,#7848,#7849,#7850,#7851,#7852,#7853));
#8170=CLOSED_SHELL('',(#7854,#7855,#7856,#7857,#7858,#7859,#7860,#7861,
#7862,#7863,#7864,#7865,#7866,#7867,#7868,#7869,#7870,#7871,#7872));
#8171=CLOSED_SHELL('',(#7873,#7874,#7875,#7876,#7877,#7878,#7879,#7880,
#7881,#7882,#7883,#7884,#7885,#7886,#7887,#7888,#7889,#7890,#7891,#7892));
#8172=CLOSED_SHELL('',(#7893,#7894,#7895,#7896,#7897,#7898,#7899,#7900,
#7901,#7902,#7903,#7904,#7905,#7906,#7907,#7908,#7909,#7910,#7911,#7912));
#8173=CLOSED_SHELL('',(#7913,#7914,#7915,#7916,#7917,#7918,#7919,#7920,
#7921,#7922,#7923,#7924,#7925,#7926,#7927,#7928,#7929,#7930,#7931,#7932,
#7933,#7934,#7935,#7936,#7937,#7938,#7939,#7940,#7941,#7942,#7943,#7944,
#7945,#7946,#7947,#7948,#7949,#7950,#7951,#7952,#7953,#7954,#7955,#7956,
#7957,#7958,#7959,#7960,#7961,#7962,#7963,#7964,#7965,#7966,#7967,#7968,
#7969,#7970,#7971,#7972,#7973,#7974,#7975,#7976,#7977,#7978,#7979,#7980,
#7981,#7982,#7983,#7984,#7985,#7986,#7987,#7988,#7989,#7990,#7991,#7992,
#7993,#7994,#7995,#7996,#7997,#7998,#7999,#8000,#8001,#8002,#8003,#8004,
#8005,#8006,#8007,#8008,#8009,#8010,#8011,#8012,#8013,#8014,#8015,#8016,
#8017,#8018,#8019,#8020,#8021,#8022,#8023,#8024,#8025,#8026,#8027,#8028,
#8029,#8030,#8031,#8032,#8033,#8034,#8035,#8036,#8037,#8038,#8039,#8040,
#8041,#8042,#8043,#8044,#8045,#8046,#8047,#8048,#8049,#8050,#8051,#8052,
#8053,#8054,#8055,#8056,#8057,#8058,#8059,#8060,#8061,#8062,#8063,#8064,
#8065,#8066,#8067,#8068,#8069,#8070,#8071,#8072,#8073,#8074,#8075,#8076,
#8077,#8078,#8079,#8080,#8081,#8082,#8083,#8084,#8085,#8086,#8087,#8088,
#8089,#8090,#8091,#8092,#8093,#8094,#8095,#8096,#8097,#8098,#8099,#8100,
#8101,#8102,#8103,#8104,#8105,#8106,#8107,#8108,#8109,#8110,#8111,#8112,
#8113,#8114,#8115,#8116,#8117,#8118,#8119,#8120,#8121,#8122,#8123,#8124,
#8125,#8126,#8127,#8128,#8129,#8130,#8131,#8132,#8133,#8134,#8135,#8136,
#8137,#8138,#8139,#8140,#8141,#8142,#8143,#8144,#8145,#8146,#8147,#8148,
#8149,#8150,#8151,#8152,#8153,#8154,#8155,#8156,#8157,#8158,#8159,#8160,
#8161,#8162,#8163,#8164,#8165,#8166,#8167));
#8174=STYLED_ITEM('',(#8180),#8219);
#8175=STYLED_ITEM('',(#8181),#8220);
#8176=STYLED_ITEM('',(#8182),#8221);
#8177=STYLED_ITEM('',(#8183),#8222);
#8178=STYLED_ITEM('',(#8184),#8223);
#8179=STYLED_ITEM('',(#8185),#8224);
#8180=PRESENTATION_STYLE_ASSIGNMENT((#8186));
#8181=PRESENTATION_STYLE_ASSIGNMENT((#8187));
#8182=PRESENTATION_STYLE_ASSIGNMENT((#8188));
#8183=PRESENTATION_STYLE_ASSIGNMENT((#8189));
#8184=PRESENTATION_STYLE_ASSIGNMENT((#8190));
#8185=PRESENTATION_STYLE_ASSIGNMENT((#8191));
#8186=SURFACE_STYLE_USAGE(.BOTH.,#8192);
#8187=SURFACE_STYLE_USAGE(.BOTH.,#8193);
#8188=SURFACE_STYLE_USAGE(.BOTH.,#8194);
#8189=SURFACE_STYLE_USAGE(.BOTH.,#8195);
#8190=SURFACE_STYLE_USAGE(.BOTH.,#8196);
#8191=SURFACE_STYLE_USAGE(.BOTH.,#8197);
#8192=SURFACE_SIDE_STYLE('',(#8198));
#8193=SURFACE_SIDE_STYLE('',(#8199));
#8194=SURFACE_SIDE_STYLE('',(#8200));
#8195=SURFACE_SIDE_STYLE('',(#8201));
#8196=SURFACE_SIDE_STYLE('',(#8202));
#8197=SURFACE_SIDE_STYLE('',(#8203));
#8198=SURFACE_STYLE_FILL_AREA(#8204);
#8199=SURFACE_STYLE_FILL_AREA(#8205);
#8200=SURFACE_STYLE_FILL_AREA(#8206);
#8201=SURFACE_STYLE_FILL_AREA(#8207);
#8202=SURFACE_STYLE_FILL_AREA(#8208);
#8203=SURFACE_STYLE_FILL_AREA(#8209);
#8204=FILL_AREA_STYLE('',(#8210));
#8205=FILL_AREA_STYLE('',(#8211));
#8206=FILL_AREA_STYLE('',(#8212));
#8207=FILL_AREA_STYLE('',(#8213));
#8208=FILL_AREA_STYLE('',(#8214));
#8209=FILL_AREA_STYLE('',(#8215));
#8210=FILL_AREA_STYLE_COLOUR('',#8216);
#8211=FILL_AREA_STYLE_COLOUR('',#8216);
#8212=FILL_AREA_STYLE_COLOUR('',#8216);
#8213=FILL_AREA_STYLE_COLOUR('',#8217);
#8214=FILL_AREA_STYLE_COLOUR('',#8217);
#8215=FILL_AREA_STYLE_COLOUR('',#8218);
#8216=COLOUR_RGB('', 0.66274510, 0.83137255, 0.94901961);
#8217=COLOUR_RGB('', 0.72549020, 0.75294118, 0.79215686);
#8218=COLOUR_RGB('', 0.09019608, 0.27058824, 0.51372549);
#8219=MANIFOLD_SOLID_BREP('cassette body__ DE    15749',#8168);
#8220=MANIFOLD_SOLID_BREP('endcap2__ DE    22113',#8169);
#8221=MANIFOLD_SOLID_BREP('endcap__ DE    14671',#8170);
#8222=MANIFOLD_SOLID_BREP(
'angular contact ball bearing_68_bsi_BS 6267 ABB - 4815 - 18,SI,NC,18_
68__ DE    23193',#8171);
#8223=MANIFOLD_SOLID_BREP(
'angular contact ball bearing_68_bsi_BS 6267 ABB - 4815 - 18,SI,NC,18_
68__ DE    23193',#8172);
#8224=MANIFOLD_SOLID_BREP('HubBody__ DE       35',#8173);
#8225=SHAPE_DEFINITION_REPRESENTATION(#18827,#8232);
#8226=SHAPE_DEFINITION_REPRESENTATION(#18828,#8233);
#8227=SHAPE_DEFINITION_REPRESENTATION(#18830,#8234);
#8228=SHAPE_DEFINITION_REPRESENTATION(#18832,#8235);
#8229=SHAPE_DEFINITION_REPRESENTATION(#18834,#8236);
#8230=SHAPE_DEFINITION_REPRESENTATION(#18836,#8237);
#8231=SHAPE_DEFINITION_REPRESENTATION(#18838,#8238);
#8232=SHAPE_REPRESENTATION('MAS-697',(#8239,#8541,#8577,#8613,#8652,#8691,
#9191),#18810);
#8233=SHAPE_REPRESENTATION('cassette body__ DE    15749',(#8239),#18811);
#8234=SHAPE_REPRESENTATION('endcap2__ DE    22113',(#8239),#18812);
#8235=SHAPE_REPRESENTATION('endcap__ DE    14671',(#8239),#18813);
#8236=SHAPE_REPRESENTATION(
'angular contact ball bearing_68_bsi_BS 6267 ABB - 4815 - 18,SI,NC,18_
68__ DE    23193',(#8239),#18814);
#8237=SHAPE_REPRESENTATION(
'angular contact ball bearing_68_bsi_BS 6267 ABB - 4815 - 18,SI,NC,18_
68__ DE    23193',(#8239),#18815);
#8238=SHAPE_REPRESENTATION('HubBody__ DE       35',(#8239),#18816);
#8239=AXIS2_PLACEMENT_3D('',#11098,#9192,#9193);
#8240=AXIS2_PLACEMENT_3D('',#11099,#9194,#9195);
#8241=AXIS2_PLACEMENT_3D('',#11100,#9196,#9197);
#8242=AXIS2_PLACEMENT_3D('',#11102,#9198,#9199);
#8243=AXIS2_PLACEMENT_3D('',#11104,#9200,#9201);
#8244=AXIS2_PLACEMENT_3D('',#11105,#9202,#9203);
#8245=AXIS2_PLACEMENT_3D('',#11107,#9204,#9205);
#8246=AXIS2_PLACEMENT_3D('',#11108,#9206,#9207);
#8247=AXIS2_PLACEMENT_3D('',#11110,#9208,#9209);
#8248=AXIS2_PLACEMENT_3D('',#11111,#9210,#9211);
#8249=AXIS2_PLACEMENT_3D('',#11119,#9212,#9213);
#8250=AXIS2_PLACEMENT_3D('',#11126,#9214,#9215);
#8251=AXIS2_PLACEMENT_3D('',#11133,#9216,#9217);
#8252=AXIS2_PLACEMENT_3D('',#11140,#9218,#9219);
#8253=AXIS2_PLACEMENT_3D('',#11147,#9220,#9221);
#8254=AXIS2_PLACEMENT_3D('',#11154,#9222,#9223);
#8255=AXIS2_PLACEMENT_3D('',#11161,#9224,#9225);
#8256=AXIS2_PLACEMENT_3D('',#11168,#9226,#9227);
#8257=AXIS2_PLACEMENT_3D('',#11175,#9228,#9229);
#8258=AXIS2_PLACEMENT_3D('',#11182,#9230,#9231);
#8259=AXIS2_PLACEMENT_3D('',#11189,#9232,#9233);
#8260=AXIS2_PLACEMENT_3D('',#11196,#9234,#9235);
#8261=AXIS2_PLACEMENT_3D('',#11203,#9236,#9237);
#8262=AXIS2_PLACEMENT_3D('',#11210,#9238,#9239);
#8263=AXIS2_PLACEMENT_3D('',#11217,#9240,#9241);
#8264=AXIS2_PLACEMENT_3D('',#11224,#9242,#9243);
#8265=AXIS2_PLACEMENT_3D('',#11231,#9244,#9245);
#8266=AXIS2_PLACEMENT_3D('',#11238,#9246,#9247);
#8267=AXIS2_PLACEMENT_3D('',#11245,#9248,#9249);
#8268=AXIS2_PLACEMENT_3D('',#11252,#9250,#9251);
#8269=AXIS2_PLACEMENT_3D('',#11259,#9252,#9253);
#8270=AXIS2_PLACEMENT_3D('',#11266,#9254,#9255);
#8271=AXIS2_PLACEMENT_3D('',#11273,#9256,#9257);
#8272=AXIS2_PLACEMENT_3D('',#11280,#9258,#9259);
#8273=AXIS2_PLACEMENT_3D('',#11287,#9260,#9261);
#8274=AXIS2_PLACEMENT_3D('',#11294,#9262,#9263);
#8275=AXIS2_PLACEMENT_3D('',#11301,#9264,#9265);
#8276=AXIS2_PLACEMENT_3D('',#11308,#9266,#9267);
#8277=AXIS2_PLACEMENT_3D('',#11315,#9268,#9269);
#8278=AXIS2_PLACEMENT_3D('',#11322,#9270,#9271);
#8279=AXIS2_PLACEMENT_3D('',#11329,#9272,#9273);
#8280=AXIS2_PLACEMENT_3D('',#11336,#9274,#9275);
#8281=AXIS2_PLACEMENT_3D('',#11343,#9276,#9277);
#8282=AXIS2_PLACEMENT_3D('',#11350,#9278,#9279);
#8283=AXIS2_PLACEMENT_3D('',#11357,#9280,#9281);
#8284=AXIS2_PLACEMENT_3D('',#11364,#9282,#9283);
#8285=AXIS2_PLACEMENT_3D('',#11371,#9284,#9285);
#8286=AXIS2_PLACEMENT_3D('',#11378,#9286,#9287);
#8287=AXIS2_PLACEMENT_3D('',#11385,#9288,#9289);
#8288=AXIS2_PLACEMENT_3D('',#11391,#9290,#9291);
#8289=AXIS2_PLACEMENT_3D('',#11392,#9292,#9293);
#8290=AXIS2_PLACEMENT_3D('',#11394,#9294,#9295);
#8291=AXIS2_PLACEMENT_3D('',#11400,#9296,#9297);
#8292=AXIS2_PLACEMENT_3D('',#11406,#9298,#9299);
#8293=AXIS2_PLACEMENT_3D('',#11421,#9300,#9301);
#8294=AXIS2_PLACEMENT_3D('',#11422,#9302,#9303);
#8295=AXIS2_PLACEMENT_3D('',#11438,#9304,#9305);
#8296=AXIS2_PLACEMENT_3D('',#11453,#9306,#9307);
#8297=AXIS2_PLACEMENT_3D('',#11454,#9308,#9309);
#8298=AXIS2_PLACEMENT_3D('',#11460,#9310,#9311);
#8299=AXIS2_PLACEMENT_3D('',#11475,#9312,#9313);
#8300=AXIS2_PLACEMENT_3D('',#11481,#9314,#9315);
#8301=AXIS2_PLACEMENT_3D('',#11492,#9316,#9317);
#8302=AXIS2_PLACEMENT_3D('',#11507,#9318,#9319);
#8303=AXIS2_PLACEMENT_3D('',#11508,#9320,#9321);
#8304=AXIS2_PLACEMENT_3D('',#11514,#9322,#9323);
#8305=AXIS2_PLACEMENT_3D('',#11529,#9324,#9325);
#8306=AXIS2_PLACEMENT_3D('',#11535,#9326,#9327);
#8307=AXIS2_PLACEMENT_3D('',#11546,#9328,#9329);
#8308=AXIS2_PLACEMENT_3D('',#11561,#9330,#9331);
#8309=AXIS2_PLACEMENT_3D('',#11562,#9332,#9333);
#8310=AXIS2_PLACEMENT_3D('',#11568,#9334,#9335);
#8311=AXIS2_PLACEMENT_3D('',#11583,#9336,#9337);
#8312=AXIS2_PLACEMENT_3D('',#11589,#9338,#9339);
#8313=AXIS2_PLACEMENT_3D('',#11600,#9340,#9341);
#8314=AXIS2_PLACEMENT_3D('',#11615,#9342,#9343);
#8315=AXIS2_PLACEMENT_3D('',#11616,#9344,#9345);
#8316=AXIS2_PLACEMENT_3D('',#11622,#9346,#9347);
#8317=AXIS2_PLACEMENT_3D('',#11637,#9348,#9349);
#8318=AXIS2_PLACEMENT_3D('',#11643,#9350,#9351);
#8319=AXIS2_PLACEMENT_3D('',#11654,#9352,#9353);
#8320=AXIS2_PLACEMENT_3D('',#11669,#9354,#9355);
#8321=AXIS2_PLACEMENT_3D('',#11670,#9356,#9357);
#8322=AXIS2_PLACEMENT_3D('',#11676,#9358,#9359);
#8323=AXIS2_PLACEMENT_3D('',#11691,#9360,#9361);
#8324=AXIS2_PLACEMENT_3D('',#11697,#9362,#9363);
#8325=AXIS2_PLACEMENT_3D('',#11708,#9364,#9365);
#8326=AXIS2_PLACEMENT_3D('',#11723,#9366,#9367);
#8327=AXIS2_PLACEMENT_3D('',#11724,#9368,#9369);
#8328=AXIS2_PLACEMENT_3D('',#11730,#9370,#9371);
#8329=AXIS2_PLACEMENT_3D('',#11745,#9372,#9373);
#8330=AXIS2_PLACEMENT_3D('',#11751,#9374,#9375);
#8331=AXIS2_PLACEMENT_3D('',#11762,#9376,#9377);
#8332=AXIS2_PLACEMENT_3D('',#11777,#9378,#9379);
#8333=AXIS2_PLACEMENT_3D('',#11778,#9380,#9381);
#8334=AXIS2_PLACEMENT_3D('',#11784,#9382,#9383);
#8335=AXIS2_PLACEMENT_3D('',#11799,#9384,#9385);
#8336=AXIS2_PLACEMENT_3D('',#11805,#9386,#9387);
#8337=AXIS2_PLACEMENT_3D('',#11816,#9388,#9389);
#8338=AXIS2_PLACEMENT_3D('',#11831,#9390,#9391);
#8339=AXIS2_PLACEMENT_3D('',#11832,#9392,#9393);
#8340=AXIS2_PLACEMENT_3D('',#11838,#9394,#9395);
#8341=AXIS2_PLACEMENT_3D('',#11853,#9396,#9397);
#8342=AXIS2_PLACEMENT_3D('',#11859,#9398,#9399);
#8343=AXIS2_PLACEMENT_3D('',#11870,#9400,#9401);
#8344=AXIS2_PLACEMENT_3D('',#11885,#9402,#9403);
#8345=AXIS2_PLACEMENT_3D('',#11886,#9404,#9405);
#8346=AXIS2_PLACEMENT_3D('',#11892,#9406,#9407);
#8347=AXIS2_PLACEMENT_3D('',#11907,#9408,#9409);
#8348=AXIS2_PLACEMENT_3D('',#11913,#9410,#9411);
#8349=AXIS2_PLACEMENT_3D('',#11924,#9412,#9413);
#8350=AXIS2_PLACEMENT_3D('',#11939,#9414,#9415);
#8351=AXIS2_PLACEMENT_3D('',#11940,#9416,#9417);
#8352=AXIS2_PLACEMENT_3D('',#11946,#9418,#9419);
#8353=AXIS2_PLACEMENT_3D('',#11961,#9420,#9421);
#8354=AXIS2_PLACEMENT_3D('',#11967,#9422,#9423);
#8355=AXIS2_PLACEMENT_3D('',#11978,#9424,#9425);
#8356=AXIS2_PLACEMENT_3D('',#11993,#9426,#9427);
#8357=AXIS2_PLACEMENT_3D('',#11994,#9428,#9429);
#8358=AXIS2_PLACEMENT_3D('',#12000,#9430,#9431);
#8359=AXIS2_PLACEMENT_3D('',#12015,#9432,#9433);
#8360=AXIS2_PLACEMENT_3D('',#12021,#9434,#9435);
#8361=AXIS2_PLACEMENT_3D('',#12032,#9436,#9437);
#8362=AXIS2_PLACEMENT_3D('',#12047,#9438,#9439);
#8363=AXIS2_PLACEMENT_3D('',#12048,#9440,#9441);
#8364=AXIS2_PLACEMENT_3D('',#12054,#9442,#9443);
#8365=AXIS2_PLACEMENT_3D('',#12069,#9444,#9445);
#8366=AXIS2_PLACEMENT_3D('',#12075,#9446,#9447);
#8367=AXIS2_PLACEMENT_3D('',#12086,#9448,#9449);
#8368=AXIS2_PLACEMENT_3D('',#12101,#9450,#9451);
#8369=AXIS2_PLACEMENT_3D('',#12102,#9452,#9453);
#8370=AXIS2_PLACEMENT_3D('',#12108,#9454,#9455);
#8371=AXIS2_PLACEMENT_3D('',#12123,#9456,#9457);
#8372=AXIS2_PLACEMENT_3D('',#12129,#9458,#9459);
#8373=AXIS2_PLACEMENT_3D('',#12140,#9460,#9461);
#8374=AXIS2_PLACEMENT_3D('',#12155,#9462,#9463);
#8375=AXIS2_PLACEMENT_3D('',#12156,#9464,#9465);
#8376=AXIS2_PLACEMENT_3D('',#12162,#9466,#9467);
#8377=AXIS2_PLACEMENT_3D('',#12177,#9468,#9469);
#8378=AXIS2_PLACEMENT_3D('',#12183,#9470,#9471);
#8379=AXIS2_PLACEMENT_3D('',#12194,#9472,#9473);
#8380=AXIS2_PLACEMENT_3D('',#12209,#9474,#9475);
#8381=AXIS2_PLACEMENT_3D('',#12210,#9476,#9477);
#8382=AXIS2_PLACEMENT_3D('',#12216,#9478,#9479);
#8383=AXIS2_PLACEMENT_3D('',#12231,#9480,#9481);
#8384=AXIS2_PLACEMENT_3D('',#12237,#9482,#9483);
#8385=AXIS2_PLACEMENT_3D('',#12248,#9484,#9485);
#8386=AXIS2_PLACEMENT_3D('',#12263,#9486,#9487);
#8387=AXIS2_PLACEMENT_3D('',#12264,#9488,#9489);
#8388=AXIS2_PLACEMENT_3D('',#12270,#9490,#9491);
#8389=AXIS2_PLACEMENT_3D('',#12285,#9492,#9493);
#8390=AXIS2_PLACEMENT_3D('',#12291,#9494,#9495);
#8391=AXIS2_PLACEMENT_3D('',#12302,#9496,#9497);
#8392=AXIS2_PLACEMENT_3D('',#12317,#9498,#9499);
#8393=AXIS2_PLACEMENT_3D('',#12318,#9500,#9501);
#8394=AXIS2_PLACEMENT_3D('',#12324,#9502,#9503);
#8395=AXIS2_PLACEMENT_3D('',#12339,#9504,#9505);
#8396=AXIS2_PLACEMENT_3D('',#12345,#9506,#9507);
#8397=AXIS2_PLACEMENT_3D('',#12356,#9508,#9509);
#8398=AXIS2_PLACEMENT_3D('',#12371,#9510,#9511);
#8399=AXIS2_PLACEMENT_3D('',#12372,#9512,#9513);
#8400=AXIS2_PLACEMENT_3D('',#12378,#9514,#9515);
#8401=AXIS2_PLACEMENT_3D('',#12393,#9516,#9517);
#8402=AXIS2_PLACEMENT_3D('',#12399,#9518,#9519);
#8403=AXIS2_PLACEMENT_3D('',#12410,#9520,#9521);
#8404=AXIS2_PLACEMENT_3D('',#12425,#9522,#9523);
#8405=AXIS2_PLACEMENT_3D('',#12426,#9524,#9525);
#8406=AXIS2_PLACEMENT_3D('',#12432,#9526,#9527);
#8407=AXIS2_PLACEMENT_3D('',#12447,#9528,#9529);
#8408=AXIS2_PLACEMENT_3D('',#12453,#9530,#9531);
#8409=AXIS2_PLACEMENT_3D('',#12464,#9532,#9533);
#8410=AXIS2_PLACEMENT_3D('',#12474,#9534,#9535);
#8411=AXIS2_PLACEMENT_3D('',#12475,#9536,#9537);
#8412=AXIS2_PLACEMENT_3D('',#12477,#9538,#9539);
#8413=AXIS2_PLACEMENT_3D('',#12478,#9540,#9541);
#8414=AXIS2_PLACEMENT_3D('',#12479,#9542,#9543);
#8415=AXIS2_PLACEMENT_3D('',#12489,#9544,#9545);
#8416=AXIS2_PLACEMENT_3D('',#12499,#9546,#9547);
#8417=AXIS2_PLACEMENT_3D('',#12505,#9548,#9549);
#8418=AXIS2_PLACEMENT_3D('',#12516,#9550,#9551);
#8419=AXIS2_PLACEMENT_3D('',#12527,#9552,#9553);
#8420=AXIS2_PLACEMENT_3D('',#12538,#9554,#9555);
#8421=AXIS2_PLACEMENT_3D('',#12549,#9556,#9557);
#8422=AXIS2_PLACEMENT_3D('',#12560,#9558,#9559);
#8423=AXIS2_PLACEMENT_3D('',#12571,#9560,#9561);
#8424=AXIS2_PLACEMENT_3D('',#12582,#9562,#9563);
#8425=AXIS2_PLACEMENT_3D('',#12593,#9564,#9565);
#8426=AXIS2_PLACEMENT_3D('',#12604,#9566,#9567);
#8427=AXIS2_PLACEMENT_3D('',#12605,#9568,#9569);
#8428=AXIS2_PLACEMENT_3D('',#12616,#9570,#9571);
#8429=AXIS2_PLACEMENT_3D('',#12627,#9572,#9573);
#8430=AXIS2_PLACEMENT_3D('',#12638,#9574,#9575);
#8431=AXIS2_PLACEMENT_3D('',#12649,#9576,#9577);
#8432=AXIS2_PLACEMENT_3D('',#12660,#9578,#9579);
#8433=AXIS2_PLACEMENT_3D('',#12671,#9580,#9581);
#8434=AXIS2_PLACEMENT_3D('',#12682,#9582,#9583);
#8435=AXIS2_PLACEMENT_3D('',#12693,#9584,#9585);
#8436=AXIS2_PLACEMENT_3D('',#12704,#9586,#9587);
#8437=AXIS2_PLACEMENT_3D('',#12710,#9588,#9589);
#8438=AXIS2_PLACEMENT_3D('',#12712,#9590,#9591);
#8439=AXIS2_PLACEMENT_3D('',#12713,#9592,#9593);
#8440=AXIS2_PLACEMENT_3D('',#12714,#9594,#9595);
#8441=AXIS2_PLACEMENT_3D('',#12719,#9596,#9597);
#8442=AXIS2_PLACEMENT_3D('',#12724,#9598,#9599);
#8443=AXIS2_PLACEMENT_3D('',#12725,#9600,#9601);
#8444=AXIS2_PLACEMENT_3D('',#12726,#9602,#9603);
#8445=AXIS2_PLACEMENT_3D('',#12731,#9604,#9605);
#8446=AXIS2_PLACEMENT_3D('',#12736,#9606,#9607);
#8447=AXIS2_PLACEMENT_3D('',#12737,#9608,#9609);
#8448=AXIS2_PLACEMENT_3D('',#12738,#9610,#9611);
#8449=AXIS2_PLACEMENT_3D('',#12743,#9612,#9613);
#8450=AXIS2_PLACEMENT_3D('',#12748,#9614,#9615);
#8451=AXIS2_PLACEMENT_3D('',#12749,#9616,#9617);
#8452=AXIS2_PLACEMENT_3D('',#12750,#9618,#9619);
#8453=AXIS2_PLACEMENT_3D('',#12755,#9620,#9621);
#8454=AXIS2_PLACEMENT_3D('',#12760,#9622,#9623);
#8455=AXIS2_PLACEMENT_3D('',#12761,#9624,#9625);
#8456=AXIS2_PLACEMENT_3D('',#12762,#9626,#9627);
#8457=AXIS2_PLACEMENT_3D('',#12767,#9628,#9629);
#8458=AXIS2_PLACEMENT_3D('',#12772,#9630,#9631);
#8459=AXIS2_PLACEMENT_3D('',#12773,#9632,#9633);
#8460=AXIS2_PLACEMENT_3D('',#12774,#9634,#9635);
#8461=AXIS2_PLACEMENT_3D('',#12779,#9636,#9637);
#8462=AXIS2_PLACEMENT_3D('',#12784,#9638,#9639);
#8463=AXIS2_PLACEMENT_3D('',#12785,#9640,#9641);
#8464=AXIS2_PLACEMENT_3D('',#12786,#9642,#9643);
#8465=AXIS2_PLACEMENT_3D('',#12791,#9644,#9645);
#8466=AXIS2_PLACEMENT_3D('',#12796,#9646,#9647);
#8467=AXIS2_PLACEMENT_3D('',#12797,#9648,#9649);
#8468=AXIS2_PLACEMENT_3D('',#12798,#9650,#9651);
#8469=AXIS2_PLACEMENT_3D('',#12803,#9652,#9653);
#8470=AXIS2_PLACEMENT_3D('',#12808,#9654,#9655);
#8471=AXIS2_PLACEMENT_3D('',#12809,#9656,#9657);
#8472=AXIS2_PLACEMENT_3D('',#12810,#9658,#9659);
#8473=AXIS2_PLACEMENT_3D('',#12815,#9660,#9661);
#8474=AXIS2_PLACEMENT_3D('',#12820,#9662,#9663);
#8475=AXIS2_PLACEMENT_3D('',#12821,#9664,#9665);
#8476=AXIS2_PLACEMENT_3D('',#12822,#9666,#9667);
#8477=AXIS2_PLACEMENT_3D('',#12827,#9668,#9669);
#8478=AXIS2_PLACEMENT_3D('',#12832,#9670,#9671);
#8479=AXIS2_PLACEMENT_3D('',#12833,#9672,#9673);
#8480=AXIS2_PLACEMENT_3D('',#12834,#9674,#9675);
#8481=AXIS2_PLACEMENT_3D('',#12839,#9676,#9677);
#8482=AXIS2_PLACEMENT_3D('',#12844,#9678,#9679);
#8483=AXIS2_PLACEMENT_3D('',#12845,#9680,#9681);
#8484=AXIS2_PLACEMENT_3D('',#12846,#9682,#9683);
#8485=AXIS2_PLACEMENT_3D('',#12851,#9684,#9685);
#8486=AXIS2_PLACEMENT_3D('',#12856,#9686,#9687);
#8487=AXIS2_PLACEMENT_3D('',#12857,#9688,#9689);
#8488=AXIS2_PLACEMENT_3D('',#12858,#9690,#9691);
#8489=AXIS2_PLACEMENT_3D('',#12863,#9692,#9693);
#8490=AXIS2_PLACEMENT_3D('',#12868,#9694,#9695);
#8491=AXIS2_PLACEMENT_3D('',#12869,#9696,#9697);
#8492=AXIS2_PLACEMENT_3D('',#12870,#9698,#9699);
#8493=AXIS2_PLACEMENT_3D('',#12875,#9700,#9701);
#8494=AXIS2_PLACEMENT_3D('',#12880,#9702,#9703);
#8495=AXIS2_PLACEMENT_3D('',#12881,#9704,#9705);
#8496=AXIS2_PLACEMENT_3D('',#12882,#9706,#9707);
#8497=AXIS2_PLACEMENT_3D('',#12887,#9708,#9709);
#8498=AXIS2_PLACEMENT_3D('',#12892,#9710,#9711);
#8499=AXIS2_PLACEMENT_3D('',#12893,#9712,#9713);
#8500=AXIS2_PLACEMENT_3D('',#12894,#9714,#9715);
#8501=AXIS2_PLACEMENT_3D('',#12899,#9716,#9717);
#8502=AXIS2_PLACEMENT_3D('',#12904,#9718,#9719);
#8503=AXIS2_PLACEMENT_3D('',#12905,#9720,#9721);
#8504=AXIS2_PLACEMENT_3D('',#12906,#9722,#9723);
#8505=AXIS2_PLACEMENT_3D('',#12911,#9724,#9725);
#8506=AXIS2_PLACEMENT_3D('',#12916,#9726,#9727);
#8507=AXIS2_PLACEMENT_3D('',#12917,#9728,#9729);
#8508=AXIS2_PLACEMENT_3D('',#12918,#9730,#9731);
#8509=AXIS2_PLACEMENT_3D('',#12923,#9732,#9733);
#8510=AXIS2_PLACEMENT_3D('',#12928,#9734,#9735);
#8511=AXIS2_PLACEMENT_3D('',#12929,#9736,#9737);
#8512=AXIS2_PLACEMENT_3D('',#12930,#9738,#9739);
#8513=AXIS2_PLACEMENT_3D('',#12935,#9740,#9741);
#8514=AXIS2_PLACEMENT_3D('',#12940,#9742,#9743);
#8515=AXIS2_PLACEMENT_3D('',#12941,#9744,#9745);
#8516=AXIS2_PLACEMENT_3D('',#12943,#9746,#9747);
#8517=AXIS2_PLACEMENT_3D('',#12944,#9748,#9749);
#8518=AXIS2_PLACEMENT_3D('',#12945,#9750,#9751);
#8519=AXIS2_PLACEMENT_3D('',#12946,#9752,#9753);
#8520=AXIS2_PLACEMENT_3D('',#12948,#9754,#9755);
#8521=AXIS2_PLACEMENT_3D('',#12949,#9756,#9757);
#8522=AXIS2_PLACEMENT_3D('',#12950,#9758,#9759);
#8523=AXIS2_PLACEMENT_3D('',#12951,#9760,#9761);
#8524=AXIS2_PLACEMENT_3D('',#12952,#9762,#9763);
#8525=AXIS2_PLACEMENT_3D('',#12953,#9764,#9765);
#8526=AXIS2_PLACEMENT_3D('',#12954,#9766,#9767);
#8527=AXIS2_PLACEMENT_3D('',#12955,#9768,#9769);
#8528=AXIS2_PLACEMENT_3D('',#12956,#9770,#9771);
#8529=AXIS2_PLACEMENT_3D('',#12957,#9772,#9773);
#8530=AXIS2_PLACEMENT_3D('',#12958,#9774,#9775);
#8531=AXIS2_PLACEMENT_3D('',#12959,#9776,#9777);
#8532=AXIS2_PLACEMENT_3D('',#12960,#9778,#9779);
#8533=AXIS2_PLACEMENT_3D('',#12961,#9780,#9781);
#8534=AXIS2_PLACEMENT_3D('',#12962,#9782,#9783);
#8535=AXIS2_PLACEMENT_3D('',#12963,#9784,#9785);
#8536=AXIS2_PLACEMENT_3D('',#12964,#9786,#9787);
#8537=AXIS2_PLACEMENT_3D('',#12965,#9788,#9789);
#8538=AXIS2_PLACEMENT_3D('',#12966,#9790,#9791);
#8539=AXIS2_PLACEMENT_3D('',#12967,#9792,#9793);
#8540=AXIS2_PLACEMENT_3D('',#12969,#9794,#9795);
#8541=AXIS2_PLACEMENT_3D('',#12970,#9796,#9797);
#8542=AXIS2_PLACEMENT_3D('',#12971,#9798,#9799);
#8543=AXIS2_PLACEMENT_3D('',#12972,#9800,#9801);
#8544=AXIS2_PLACEMENT_3D('',#12974,#9802,#9803);
#8545=AXIS2_PLACEMENT_3D('',#12976,#9804,#9805);
#8546=AXIS2_PLACEMENT_3D('',#12977,#9806,#9807);
#8547=AXIS2_PLACEMENT_3D('',#12979,#9808,#9809);
#8548=AXIS2_PLACEMENT_3D('',#12980,#9810,#9811);
#8549=AXIS2_PLACEMENT_3D('',#12982,#9812,#9813);
#8550=AXIS2_PLACEMENT_3D('',#12983,#9814,#9815);
#8551=AXIS2_PLACEMENT_3D('',#12997,#9816,#9817);
#8552=AXIS2_PLACEMENT_3D('',#12998,#9818,#9819);
#8553=AXIS2_PLACEMENT_3D('',#13000,#9820,#9821);
#8554=AXIS2_PLACEMENT_3D('',#13014,#9822,#9823);
#8555=AXIS2_PLACEMENT_3D('',#13015,#9824,#9825);
#8556=AXIS2_PLACEMENT_3D('',#13025,#9826,#9827);
#8557=AXIS2_PLACEMENT_3D('',#13026,#9828,#9829);
#8558=AXIS2_PLACEMENT_3D('',#13027,#9830,#9831);
#8559=AXIS2_PLACEMENT_3D('',#13029,#9832,#9833);
#8560=AXIS2_PLACEMENT_3D('',#13039,#9834,#9835);
#8561=AXIS2_PLACEMENT_3D('',#13040,#9836,#9837);
#8562=AXIS2_PLACEMENT_3D('',#13041,#9838,#9839);
#8563=AXIS2_PLACEMENT_3D('',#13055,#9840,#9841);
#8564=AXIS2_PLACEMENT_3D('',#13073,#9842,#9843);
#8565=AXIS2_PLACEMENT_3D('',#13074,#9844,#9845);
#8566=AXIS2_PLACEMENT_3D('',#13075,#9846,#9847);
#8567=AXIS2_PLACEMENT_3D('',#13089,#9848,#9849);
#8568=AXIS2_PLACEMENT_3D('',#13090,#9850,#9851);
#8569=AXIS2_PLACEMENT_3D('',#13091,#9852,#9853);
#8570=AXIS2_PLACEMENT_3D('',#13105,#9854,#9855);
#8571=AXIS2_PLACEMENT_3D('',#13111,#9856,#9857);
#8572=AXIS2_PLACEMENT_3D('',#13117,#9858,#9859);
#8573=AXIS2_PLACEMENT_3D('',#13129,#9860,#9861);
#8574=AXIS2_PLACEMENT_3D('',#13151,#9862,#9863);
#8575=AXIS2_PLACEMENT_3D('',#13152,#9864,#9865);
#8576=AXIS2_PLACEMENT_3D('',#13153,#9866,#9867);
#8577=AXIS2_PLACEMENT_3D('',#13154,#9868,#9869);
#8578=AXIS2_PLACEMENT_3D('',#13155,#9870,#9871);
#8579=AXIS2_PLACEMENT_3D('',#13156,#9872,#9873);
#8580=AXIS2_PLACEMENT_3D('',#13158,#9874,#9875);
#8581=AXIS2_PLACEMENT_3D('',#13160,#9876,#9877);
#8582=AXIS2_PLACEMENT_3D('',#13161,#9878,#9879);
#8583=AXIS2_PLACEMENT_3D('',#13163,#9880,#9881);
#8584=AXIS2_PLACEMENT_3D('',#13164,#9882,#9883);
#8585=AXIS2_PLACEMENT_3D('',#13166,#9884,#9885);
#8586=AXIS2_PLACEMENT_3D('',#13167,#9886,#9887);
#8587=AXIS2_PLACEMENT_3D('',#13181,#9888,#9889);
#8588=AXIS2_PLACEMENT_3D('',#13182,#9890,#9891);
#8589=AXIS2_PLACEMENT_3D('',#13184,#9892,#9893);
#8590=AXIS2_PLACEMENT_3D('',#13198,#9894,#9895);
#8591=AXIS2_PLACEMENT_3D('',#13199,#9896,#9897);
#8592=AXIS2_PLACEMENT_3D('',#13209,#9898,#9899);
#8593=AXIS2_PLACEMENT_3D('',#13210,#9900,#9901);
#8594=AXIS2_PLACEMENT_3D('',#13211,#9902,#9903);
#8595=AXIS2_PLACEMENT_3D('',#13213,#9904,#9905);
#8596=AXIS2_PLACEMENT_3D('',#13223,#9906,#9907);
#8597=AXIS2_PLACEMENT_3D('',#13224,#9908,#9909);
#8598=AXIS2_PLACEMENT_3D('',#13225,#9910,#9911);
#8599=AXIS2_PLACEMENT_3D('',#13239,#9912,#9913);
#8600=AXIS2_PLACEMENT_3D('',#13257,#9914,#9915);
#8601=AXIS2_PLACEMENT_3D('',#13258,#9916,#9917);
#8602=AXIS2_PLACEMENT_3D('',#13259,#9918,#9919);
#8603=AXIS2_PLACEMENT_3D('',#13273,#9920,#9921);
#8604=AXIS2_PLACEMENT_3D('',#13274,#9922,#9923);
#8605=AXIS2_PLACEMENT_3D('',#13275,#9924,#9925);
#8606=AXIS2_PLACEMENT_3D('',#13289,#9926,#9927);
#8607=AXIS2_PLACEMENT_3D('',#13295,#9928,#9929);
#8608=AXIS2_PLACEMENT_3D('',#13301,#9930,#9931);
#8609=AXIS2_PLACEMENT_3D('',#13313,#9932,#9933);
#8610=AXIS2_PLACEMENT_3D('',#13335,#9934,#9935);
#8611=AXIS2_PLACEMENT_3D('',#13336,#9936,#9937);
#8612=AXIS2_PLACEMENT_3D('',#13337,#9938,#9939);
#8613=AXIS2_PLACEMENT_3D('',#13338,#9940,#9941);
#8614=AXIS2_PLACEMENT_3D('',#13339,#9942,#9943);
#8615=AXIS2_PLACEMENT_3D('',#13353,#9944,#9945);
#8616=AXIS2_PLACEMENT_3D('',#13354,#9946,#9947);
#8617=AXIS2_PLACEMENT_3D('',#13356,#9948,#9949);
#8618=AXIS2_PLACEMENT_3D('',#13357,#9950,#9951);
#8619=AXIS2_PLACEMENT_3D('',#13359,#9952,#9953);
#8620=AXIS2_PLACEMENT_3D('',#13373,#9954,#9955);
#8621=AXIS2_PLACEMENT_3D('',#13374,#9956,#9957);
#8622=AXIS2_PLACEMENT_3D('',#13388,#9958,#9959);
#8623=AXIS2_PLACEMENT_3D('',#13389,#9960,#9961);
#8624=AXIS2_PLACEMENT_3D('',#13390,#9962,#9963);
#8625=AXIS2_PLACEMENT_3D('',#13392,#9964,#9965);
#8626=AXIS2_PLACEMENT_3D('',#13416,#9966,#9967);
#8627=AXIS2_PLACEMENT_3D('',#13417,#9968,#9969);
#8628=AXIS2_PLACEMENT_3D('',#13418,#9970,#9971);
#8629=AXIS2_PLACEMENT_3D('',#13419,#9972,#9973);
#8630=AXIS2_PLACEMENT_3D('',#13421,#9974,#9975);
#8631=AXIS2_PLACEMENT_3D('',#13422,#9976,#9977);
#8632=AXIS2_PLACEMENT_3D('',#13424,#9978,#9979);
#8633=AXIS2_PLACEMENT_3D('',#13438,#9980,#9981);
#8634=AXIS2_PLACEMENT_3D('',#13439,#9982,#9983);
#8635=AXIS2_PLACEMENT_3D('',#13440,#9984,#9985);
#8636=AXIS2_PLACEMENT_3D('',#13443,#9986,#9987);
#8637=AXIS2_PLACEMENT_3D('',#13444,#9988,#9989);
#8638=AXIS2_PLACEMENT_3D('',#13468,#9990,#9991);
#8639=AXIS2_PLACEMENT_3D('',#13469,#9992,#9993);
#8640=AXIS2_PLACEMENT_3D('',#13470,#9994,#9995);
#8641=AXIS2_PLACEMENT_3D('',#13488,#9996,#9997);
#8642=AXIS2_PLACEMENT_3D('',#13489,#9998,#9999);
#8643=AXIS2_PLACEMENT_3D('',#13490,#10000,#10001);
#8644=AXIS2_PLACEMENT_3D('',#13491,#10002,#10003);
#8645=AXIS2_PLACEMENT_3D('',#13493,#10004,#10005);
#8646=AXIS2_PLACEMENT_3D('',#13503,#10006,#10007);
#8647=AXIS2_PLACEMENT_3D('',#13504,#10008,#10009);
#8648=AXIS2_PLACEMENT_3D('',#13505,#10010,#10011);
#8649=AXIS2_PLACEMENT_3D('',#13508,#10012,#10013);
#8650=AXIS2_PLACEMENT_3D('',#13509,#10014,#10015);
#8651=AXIS2_PLACEMENT_3D('',#13518,#10016,#10017);
#8652=AXIS2_PLACEMENT_3D('',#13519,#10018,#10019);
#8653=AXIS2_PLACEMENT_3D('',#13520,#10020,#10021);
#8654=AXIS2_PLACEMENT_3D('',#13534,#10022,#10023);
#8655=AXIS2_PLACEMENT_3D('',#13535,#10024,#10025);
#8656=AXIS2_PLACEMENT_3D('',#13537,#10026,#10027);
#8657=AXIS2_PLACEMENT_3D('',#13538,#10028,#10029);
#8658=AXIS2_PLACEMENT_3D('',#13540,#10030,#10031);
#8659=AXIS2_PLACEMENT_3D('',#13554,#10032,#10033);
#8660=AXIS2_PLACEMENT_3D('',#13555,#10034,#10035);
#8661=AXIS2_PLACEMENT_3D('',#13569,#10036,#10037);
#8662=AXIS2_PLACEMENT_3D('',#13570,#10038,#10039);
#8663=AXIS2_PLACEMENT_3D('',#13571,#10040,#10041);
#8664=AXIS2_PLACEMENT_3D('',#13573,#10042,#10043);
#8665=AXIS2_PLACEMENT_3D('',#13597,#10044,#10045);
#8666=AXIS2_PLACEMENT_3D('',#13598,#10046,#10047);
#8667=AXIS2_PLACEMENT_3D('',#13599,#10048,#10049);
#8668=AXIS2_PLACEMENT_3D('',#13600,#10050,#10051);
#8669=AXIS2_PLACEMENT_3D('',#13602,#10052,#10053);
#8670=AXIS2_PLACEMENT_3D('',#13603,#10054,#10055);
#8671=AXIS2_PLACEMENT_3D('',#13605,#10056,#10057);
#8672=AXIS2_PLACEMENT_3D('',#13619,#10058,#10059);
#8673=AXIS2_PLACEMENT_3D('',#13620,#10060,#10061);
#8674=AXIS2_PLACEMENT_3D('',#13621,#10062,#10063);
#8675=AXIS2_PLACEMENT_3D('',#13624,#10064,#10065);
#8676=AXIS2_PLACEMENT_3D('',#13625,#10066,#10067);
#8677=AXIS2_PLACEMENT_3D('',#13649,#10068,#10069);
#8678=AXIS2_PLACEMENT_3D('',#13650,#10070,#10071);
#8679=AXIS2_PLACEMENT_3D('',#13651,#10072,#10073);
#8680=AXIS2_PLACEMENT_3D('',#13669,#10074,#10075);
#8681=AXIS2_PLACEMENT_3D('',#13670,#10076,#10077);
#8682=AXIS2_PLACEMENT_3D('',#13671,#10078,#10079);
#8683=AXIS2_PLACEMENT_3D('',#13672,#10080,#10081);
#8684=AXIS2_PLACEMENT_3D('',#13674,#10082,#10083);
#8685=AXIS2_PLACEMENT_3D('',#13684,#10084,#10085);
#8686=AXIS2_PLACEMENT_3D('',#13685,#10086,#10087);
#8687=AXIS2_PLACEMENT_3D('',#13686,#10088,#10089);
#8688=AXIS2_PLACEMENT_3D('',#13689,#10090,#10091);
#8689=AXIS2_PLACEMENT_3D('',#13690,#10092,#10093);
#8690=AXIS2_PLACEMENT_3D('',#13699,#10094,#10095);
#8691=AXIS2_PLACEMENT_3D('',#13700,#10096,#10097);
#8692=AXIS2_PLACEMENT_3D('',#13701,#10098,#10099);
#8693=AXIS2_PLACEMENT_3D('',#13702,#10100,#10101);
#8694=AXIS2_PLACEMENT_3D('',#13704,#10102,#10103);
#8695=AXIS2_PLACEMENT_3D('',#13706,#10104,#10105);
#8696=AXIS2_PLACEMENT_3D('',#13707,#10106,#10107);
#8697=AXIS2_PLACEMENT_3D('',#13709,#10108,#10109);
#8698=AXIS2_PLACEMENT_3D('',#13710,#10110,#10111);
#8699=AXIS2_PLACEMENT_3D('',#13712,#10112,#10113);
#8700=AXIS2_PLACEMENT_3D('',#13713,#10114,#10115);
#8701=AXIS2_PLACEMENT_3D('',#13715,#10116,#10117);
#8702=AXIS2_PLACEMENT_3D('',#13716,#10118,#10119);
#8703=AXIS2_PLACEMENT_3D('',#13718,#10120,#10121);
#8704=AXIS2_PLACEMENT_3D('',#13719,#10122,#10123);
#8705=AXIS2_PLACEMENT_3D('',#13721,#10124,#10125);
#8706=AXIS2_PLACEMENT_3D('',#13722,#10126,#10127);
#8707=AXIS2_PLACEMENT_3D('',#13724,#10128,#10129);
#8708=AXIS2_PLACEMENT_3D('',#13725,#10130,#10131);
#8709=AXIS2_PLACEMENT_3D('',#13727,#10132,#10133);
#8710=AXIS2_PLACEMENT_3D('',#13728,#10134,#10135);
#8711=AXIS2_PLACEMENT_3D('',#13730,#10136,#10137);
#8712=AXIS2_PLACEMENT_3D('',#13731,#10138,#10139);
#8713=AXIS2_PLACEMENT_3D('',#13733,#10140,#10141);
#8714=AXIS2_PLACEMENT_3D('',#13734,#10142,#10143);
#8715=AXIS2_PLACEMENT_3D('',#13736,#10144,#10145);
#8716=AXIS2_PLACEMENT_3D('',#13737,#10146,#10147);
#8717=AXIS2_PLACEMENT_3D('',#13739,#10148,#10149);
#8718=AXIS2_PLACEMENT_3D('',#13740,#10150,#10151);
#8719=AXIS2_PLACEMENT_3D('',#13742,#10152,#10153);
#8720=AXIS2_PLACEMENT_3D('',#13743,#10154,#10155);
#8721=AXIS2_PLACEMENT_3D('',#13745,#10156,#10157);
#8722=AXIS2_PLACEMENT_3D('',#13746,#10158,#10159);
#8723=AXIS2_PLACEMENT_3D('',#13748,#10160,#10161);
#8724=AXIS2_PLACEMENT_3D('',#13749,#10162,#10163);
#8725=AXIS2_PLACEMENT_3D('',#13751,#10164,#10165);
#8726=AXIS2_PLACEMENT_3D('',#13752,#10166,#10167);
#8727=AXIS2_PLACEMENT_3D('',#13754,#10168,#10169);
#8728=AXIS2_PLACEMENT_3D('',#13755,#10170,#10171);
#8729=AXIS2_PLACEMENT_3D('',#13757,#10172,#10173);
#8730=AXIS2_PLACEMENT_3D('',#13758,#10174,#10175);
#8731=AXIS2_PLACEMENT_3D('',#13760,#10176,#10177);
#8732=AXIS2_PLACEMENT_3D('',#13761,#10178,#10179);
#8733=AXIS2_PLACEMENT_3D('',#13763,#10180,#10181);
#8734=AXIS2_PLACEMENT_3D('',#13764,#10182,#10183);
#8735=AXIS2_PLACEMENT_3D('',#13766,#10184,#10185);
#8736=AXIS2_PLACEMENT_3D('',#13767,#10186,#10187);
#8737=AXIS2_PLACEMENT_3D('',#13769,#10188,#10189);
#8738=AXIS2_PLACEMENT_3D('',#13770,#10190,#10191);
#8739=AXIS2_PLACEMENT_3D('',#13772,#10192,#10193);
#8740=AXIS2_PLACEMENT_3D('',#13773,#10194,#10195);
#8741=AXIS2_PLACEMENT_3D('',#13775,#10196,#10197);
#8742=AXIS2_PLACEMENT_3D('',#13776,#10198,#10199);
#8743=AXIS2_PLACEMENT_3D('',#13778,#10200,#10201);
#8744=AXIS2_PLACEMENT_3D('',#13779,#10202,#10203);
#8745=AXIS2_PLACEMENT_3D('',#13781,#10204,#10205);
#8746=AXIS2_PLACEMENT_3D('',#13782,#10206,#10207);
#8747=AXIS2_PLACEMENT_3D('',#13784,#10208,#10209);
#8748=AXIS2_PLACEMENT_3D('',#13785,#10210,#10211);
#8749=AXIS2_PLACEMENT_3D('',#13787,#10212,#10213);
#8750=AXIS2_PLACEMENT_3D('',#13788,#10214,#10215);
#8751=AXIS2_PLACEMENT_3D('',#13790,#10216,#10217);
#8752=AXIS2_PLACEMENT_3D('',#13791,#10218,#10219);
#8753=AXIS2_PLACEMENT_3D('',#13793,#10220,#10221);
#8754=AXIS2_PLACEMENT_3D('',#13794,#10222,#10223);
#8755=AXIS2_PLACEMENT_3D('',#13796,#10224,#10225);
#8756=AXIS2_PLACEMENT_3D('',#13797,#10226,#10227);
#8757=AXIS2_PLACEMENT_3D('',#13799,#10228,#10229);
#8758=AXIS2_PLACEMENT_3D('',#13800,#10230,#10231);
#8759=AXIS2_PLACEMENT_3D('',#13802,#10232,#10233);
#8760=AXIS2_PLACEMENT_3D('',#13803,#10234,#10235);
#8761=AXIS2_PLACEMENT_3D('',#13805,#10236,#10237);
#8762=AXIS2_PLACEMENT_3D('',#13807,#10238,#10239);
#8763=AXIS2_PLACEMENT_3D('',#13809,#10240,#10241);
#8764=AXIS2_PLACEMENT_3D('',#13811,#10242,#10243);
#8765=AXIS2_PLACEMENT_3D('',#13813,#10244,#10245);
#8766=AXIS2_PLACEMENT_3D('',#13815,#10246,#10247);
#8767=AXIS2_PLACEMENT_3D('',#13817,#10248,#10249);
#8768=AXIS2_PLACEMENT_3D('',#13819,#10250,#10251);
#8769=AXIS2_PLACEMENT_3D('',#13821,#10252,#10253);
#8770=AXIS2_PLACEMENT_3D('',#13823,#10254,#10255);
#8771=AXIS2_PLACEMENT_3D('',#13825,#10256,#10257);
#8772=AXIS2_PLACEMENT_3D('',#13827,#10258,#10259);
#8773=AXIS2_PLACEMENT_3D('',#13829,#10260,#10261);
#8774=AXIS2_PLACEMENT_3D('',#13831,#10262,#10263);
#8775=AXIS2_PLACEMENT_3D('',#13833,#10264,#10265);
#8776=AXIS2_PLACEMENT_3D('',#13835,#10266,#10267);
#8777=AXIS2_PLACEMENT_3D('',#13837,#10268,#10269);
#8778=AXIS2_PLACEMENT_3D('',#13839,#10270,#10271);
#8779=AXIS2_PLACEMENT_3D('',#13841,#10272,#10273);
#8780=AXIS2_PLACEMENT_3D('',#13842,#10274,#10275);
#8781=AXIS2_PLACEMENT_3D('',#13844,#10276,#10277);
#8782=AXIS2_PLACEMENT_3D('',#13845,#10278,#10279);
#8783=AXIS2_PLACEMENT_3D('',#13847,#10280,#10281);
#8784=AXIS2_PLACEMENT_3D('',#13848,#10282,#10283);
#8785=AXIS2_PLACEMENT_3D('',#13850,#10284,#10285);
#8786=AXIS2_PLACEMENT_3D('',#13851,#10286,#10287);
#8787=AXIS2_PLACEMENT_3D('',#13853,#10288,#10289);
#8788=AXIS2_PLACEMENT_3D('',#13854,#10290,#10291);
#8789=AXIS2_PLACEMENT_3D('',#13856,#10292,#10293);
#8790=AXIS2_PLACEMENT_3D('',#13857,#10294,#10295);
#8791=AXIS2_PLACEMENT_3D('',#13859,#10296,#10297);
#8792=AXIS2_PLACEMENT_3D('',#13860,#10298,#10299);
#8793=AXIS2_PLACEMENT_3D('',#13862,#10300,#10301);
#8794=AXIS2_PLACEMENT_3D('',#13863,#10302,#10303);
#8795=AXIS2_PLACEMENT_3D('',#13865,#10304,#10305);
#8796=AXIS2_PLACEMENT_3D('',#13866,#10306,#10307);
#8797=AXIS2_PLACEMENT_3D('',#13868,#10308,#10309);
#8798=AXIS2_PLACEMENT_3D('',#13869,#10310,#10311);
#8799=AXIS2_PLACEMENT_3D('',#13871,#10312,#10313);
#8800=AXIS2_PLACEMENT_3D('',#13872,#10314,#10315);
#8801=AXIS2_PLACEMENT_3D('',#13874,#10316,#10317);
#8802=AXIS2_PLACEMENT_3D('',#13875,#10318,#10319);
#8803=AXIS2_PLACEMENT_3D('',#13877,#10320,#10321);
#8804=AXIS2_PLACEMENT_3D('',#13878,#10322,#10323);
#8805=AXIS2_PLACEMENT_3D('',#13880,#10324,#10325);
#8806=AXIS2_PLACEMENT_3D('',#13881,#10326,#10327);
#8807=AXIS2_PLACEMENT_3D('',#13883,#10328,#10329);
#8808=AXIS2_PLACEMENT_3D('',#13884,#10330,#10331);
#8809=AXIS2_PLACEMENT_3D('',#13886,#10332,#10333);
#8810=AXIS2_PLACEMENT_3D('',#13887,#10334,#10335);
#8811=AXIS2_PLACEMENT_3D('',#13889,#10336,#10337);
#8812=AXIS2_PLACEMENT_3D('',#13890,#10338,#10339);
#8813=AXIS2_PLACEMENT_3D('',#13892,#10340,#10341);
#8814=AXIS2_PLACEMENT_3D('',#13893,#10342,#10343);
#8815=AXIS2_PLACEMENT_3D('',#13895,#10344,#10345);
#8816=AXIS2_PLACEMENT_3D('',#13896,#10346,#10347);
#8817=AXIS2_PLACEMENT_3D('',#13898,#10348,#10349);
#8818=AXIS2_PLACEMENT_3D('',#13899,#10350,#10351);
#8819=AXIS2_PLACEMENT_3D('',#13913,#10352,#10353);
#8820=AXIS2_PLACEMENT_3D('',#13914,#10354,#10355);
#8821=AXIS2_PLACEMENT_3D('',#13928,#10356,#10357);
#8822=AXIS2_PLACEMENT_3D('',#13929,#10358,#10359);
#8823=AXIS2_PLACEMENT_3D('',#13931,#10360,#10361);
#8824=AXIS2_PLACEMENT_3D('',#13933,#10362,#10363);
#8825=AXIS2_PLACEMENT_3D('',#13947,#10364,#10365);
#8826=AXIS2_PLACEMENT_3D('',#13948,#10366,#10367);
#8827=AXIS2_PLACEMENT_3D('',#13949,#10368,#10369);
#8828=AXIS2_PLACEMENT_3D('',#13963,#10370,#10371);
#8829=AXIS2_PLACEMENT_3D('',#13988,#10372,#10373);
#8830=AXIS2_PLACEMENT_3D('',#13989,#10374,#10375);
#8831=AXIS2_PLACEMENT_3D('',#13990,#10376,#10377);
#8832=AXIS2_PLACEMENT_3D('',#13992,#10378,#10379);
#8833=AXIS2_PLACEMENT_3D('',#14006,#10380,#10381);
#8834=AXIS2_PLACEMENT_3D('',#14007,#10382,#10383);
#8835=AXIS2_PLACEMENT_3D('',#14008,#10384,#10385);
#8836=AXIS2_PLACEMENT_3D('',#14010,#10386,#10387);
#8837=AXIS2_PLACEMENT_3D('',#14016,#10388,#10389);
#8838=AXIS2_PLACEMENT_3D('',#14022,#10390,#10391);
#8839=AXIS2_PLACEMENT_3D('',#14034,#10392,#10393);
#8840=AXIS2_PLACEMENT_3D('',#14035,#10394,#10395);
#8841=AXIS2_PLACEMENT_3D('',#14049,#10396,#10397);
#8842=AXIS2_PLACEMENT_3D('',#14152,#10398,#10399);
#8843=AXIS2_PLACEMENT_3D('',#14202,#10400,#10401);
#8844=AXIS2_PLACEMENT_3D('',#14246,#10402,#10403);
#8845=AXIS2_PLACEMENT_3D('',#14247,#10404,#10405);
#8846=AXIS2_PLACEMENT_3D('',#14249,#10406,#10407);
#8847=AXIS2_PLACEMENT_3D('',#14250,#10408,#10409);
#8848=AXIS2_PLACEMENT_3D('',#14278,#10410,#10411);
#8849=AXIS2_PLACEMENT_3D('',#14289,#10412,#10413);
#8850=AXIS2_PLACEMENT_3D('',#14290,#10414,#10415);
#8851=AXIS2_PLACEMENT_3D('',#14297,#10416,#10417);
#8852=AXIS2_PLACEMENT_3D('',#14316,#10418,#10419);
#8853=AXIS2_PLACEMENT_3D('',#14334,#10420,#10421);
#8854=AXIS2_PLACEMENT_3D('',#14345,#10422,#10423);
#8855=AXIS2_PLACEMENT_3D('',#14346,#10424,#10425);
#8856=AXIS2_PLACEMENT_3D('',#14353,#10426,#10427);
#8857=AXIS2_PLACEMENT_3D('',#14372,#10428,#10429);
#8858=AXIS2_PLACEMENT_3D('',#14390,#10430,#10431);
#8859=AXIS2_PLACEMENT_3D('',#14401,#10432,#10433);
#8860=AXIS2_PLACEMENT_3D('',#14402,#10434,#10435);
#8861=AXIS2_PLACEMENT_3D('',#14409,#10436,#10437);
#8862=AXIS2_PLACEMENT_3D('',#14420,#10438,#10439);
#8863=AXIS2_PLACEMENT_3D('',#14426,#10440,#10441);
#8864=AXIS2_PLACEMENT_3D('',#14427,#10442,#10443);
#8865=AXIS2_PLACEMENT_3D('',#14438,#10444,#10445);
#8866=AXIS2_PLACEMENT_3D('',#14449,#10446,#10447);
#8867=AXIS2_PLACEMENT_3D('',#14450,#10448,#10449);
#8868=AXIS2_PLACEMENT_3D('',#14457,#10450,#10451);
#8869=AXIS2_PLACEMENT_3D('',#14468,#10452,#10453);
#8870=AXIS2_PLACEMENT_3D('',#14479,#10454,#10455);
#8871=AXIS2_PLACEMENT_3D('',#14490,#10456,#10457);
#8872=AXIS2_PLACEMENT_3D('',#14491,#10458,#10459);
#8873=AXIS2_PLACEMENT_3D('',#14498,#10460,#10461);
#8874=AXIS2_PLACEMENT_3D('',#14509,#10462,#10463);
#8875=AXIS2_PLACEMENT_3D('',#14520,#10464,#10465);
#8876=AXIS2_PLACEMENT_3D('',#14531,#10466,#10467);
#8877=AXIS2_PLACEMENT_3D('',#14532,#10468,#10469);
#8878=AXIS2_PLACEMENT_3D('',#14539,#10470,#10471);
#8879=AXIS2_PLACEMENT_3D('',#14544,#10472,#10473);
#8880=AXIS2_PLACEMENT_3D('',#14545,#10474,#10475);
#8881=AXIS2_PLACEMENT_3D('',#14547,#10476,#10477);
#8882=AXIS2_PLACEMENT_3D('',#14558,#10478,#10479);
#8883=AXIS2_PLACEMENT_3D('',#14559,#10480,#10481);
#8884=AXIS2_PLACEMENT_3D('',#14560,#10482,#10483);
#8885=AXIS2_PLACEMENT_3D('',#14567,#10484,#10485);
#8886=AXIS2_PLACEMENT_3D('',#14568,#10486,#10487);
#8887=AXIS2_PLACEMENT_3D('',#14569,#10488,#10489);
#8888=AXIS2_PLACEMENT_3D('',#14577,#10490,#10491);
#8889=AXIS2_PLACEMENT_3D('',#14578,#10492,#10493);
#8890=AXIS2_PLACEMENT_3D('',#14585,#10494,#10495);
#8891=AXIS2_PLACEMENT_3D('',#14587,#10496,#10497);
#8892=AXIS2_PLACEMENT_3D('',#14589,#10498,#10499);
#8893=AXIS2_PLACEMENT_3D('',#14596,#10500,#10501);
#8894=AXIS2_PLACEMENT_3D('',#14597,#10502,#10503);
#8895=AXIS2_PLACEMENT_3D('',#14604,#10504,#10505);
#8896=AXIS2_PLACEMENT_3D('',#14606,#10506,#10507);
#8897=AXIS2_PLACEMENT_3D('',#14608,#10508,#10509);
#8898=AXIS2_PLACEMENT_3D('',#14615,#10510,#10511);
#8899=AXIS2_PLACEMENT_3D('',#14621,#10512,#10513);
#8900=AXIS2_PLACEMENT_3D('',#14623,#10514,#10515);
#8901=AXIS2_PLACEMENT_3D('',#14625,#10516,#10517);
#8902=AXIS2_PLACEMENT_3D('',#14632,#10518,#10519);
#8903=AXIS2_PLACEMENT_3D('',#14633,#10520,#10521);
#8904=AXIS2_PLACEMENT_3D('',#14640,#10522,#10523);
#8905=AXIS2_PLACEMENT_3D('',#14642,#10524,#10525);
#8906=AXIS2_PLACEMENT_3D('',#14644,#10526,#10527);
#8907=AXIS2_PLACEMENT_3D('',#14651,#10528,#10529);
#8908=AXIS2_PLACEMENT_3D('',#14652,#10530,#10531);
#8909=AXIS2_PLACEMENT_3D('',#14659,#10532,#10533);
#8910=AXIS2_PLACEMENT_3D('',#14661,#10534,#10535);
#8911=AXIS2_PLACEMENT_3D('',#14663,#10536,#10537);
#8912=AXIS2_PLACEMENT_3D('',#14670,#10538,#10539);
#8913=AXIS2_PLACEMENT_3D('',#14671,#10540,#10541);
#8914=AXIS2_PLACEMENT_3D('',#14678,#10542,#10543);
#8915=AXIS2_PLACEMENT_3D('',#14680,#10544,#10545);
#8916=AXIS2_PLACEMENT_3D('',#14682,#10546,#10547);
#8917=AXIS2_PLACEMENT_3D('',#14683,#10548,#10549);
#8918=AXIS2_PLACEMENT_3D('',#14685,#10550,#10551);
#8919=AXIS2_PLACEMENT_3D('',#14687,#10552,#10553);
#8920=AXIS2_PLACEMENT_3D('',#14689,#10554,#10555);
#8921=AXIS2_PLACEMENT_3D('',#14691,#10556,#10557);
#8922=AXIS2_PLACEMENT_3D('',#14693,#10558,#10559);
#8923=AXIS2_PLACEMENT_3D('',#14695,#10560,#10561);
#8924=AXIS2_PLACEMENT_3D('',#14697,#10562,#10563);
#8925=AXIS2_PLACEMENT_3D('',#14699,#10564,#10565);
#8926=AXIS2_PLACEMENT_3D('',#14701,#10566,#10567);
#8927=AXIS2_PLACEMENT_3D('',#14703,#10568,#10569);
#8928=AXIS2_PLACEMENT_3D('',#14705,#10570,#10571);
#8929=AXIS2_PLACEMENT_3D('',#14707,#10572,#10573);
#8930=AXIS2_PLACEMENT_3D('',#14709,#10574,#10575);
#8931=AXIS2_PLACEMENT_3D('',#14711,#10576,#10577);
#8932=AXIS2_PLACEMENT_3D('',#14713,#10578,#10579);
#8933=AXIS2_PLACEMENT_3D('',#14715,#10580,#10581);
#8934=AXIS2_PLACEMENT_3D('',#14717,#10582,#10583);
#8935=AXIS2_PLACEMENT_3D('',#14719,#10584,#10585);
#8936=AXIS2_PLACEMENT_3D('',#14725,#10586,#10587);
#8937=AXIS2_PLACEMENT_3D('',#14731,#10588,#10589);
#8938=AXIS2_PLACEMENT_3D('',#14737,#10590,#10591);
#8939=AXIS2_PLACEMENT_3D('',#14738,#10592,#10593);
#8940=AXIS2_PLACEMENT_3D('',#14739,#10594,#10595);
#8941=AXIS2_PLACEMENT_3D('',#14745,#10596,#10597);
#8942=AXIS2_PLACEMENT_3D('',#14751,#10598,#10599);
#8943=AXIS2_PLACEMENT_3D('',#14757,#10600,#10601);
#8944=AXIS2_PLACEMENT_3D('',#14758,#10602,#10603);
#8945=AXIS2_PLACEMENT_3D('',#14764,#10604,#10605);
#8946=AXIS2_PLACEMENT_3D('',#14765,#10606,#10607);
#8947=AXIS2_PLACEMENT_3D('',#14771,#10608,#10609);
#8948=AXIS2_PLACEMENT_3D('',#14777,#10610,#10611);
#8949=AXIS2_PLACEMENT_3D('',#14783,#10612,#10613);
#8950=AXIS2_PLACEMENT_3D('',#14784,#10614,#10615);
#8951=AXIS2_PLACEMENT_3D('',#14790,#10616,#10617);
#8952=AXIS2_PLACEMENT_3D('',#14791,#10618,#10619);
#8953=AXIS2_PLACEMENT_3D('',#14797,#10620,#10621);
#8954=AXIS2_PLACEMENT_3D('',#14803,#10622,#10623);
#8955=AXIS2_PLACEMENT_3D('',#14809,#10624,#10625);
#8956=AXIS2_PLACEMENT_3D('',#14810,#10626,#10627);
#8957=AXIS2_PLACEMENT_3D('',#14816,#10628,#10629);
#8958=AXIS2_PLACEMENT_3D('',#14817,#10630,#10631);
#8959=AXIS2_PLACEMENT_3D('',#14823,#10632,#10633);
#8960=AXIS2_PLACEMENT_3D('',#14829,#10634,#10635);
#8961=AXIS2_PLACEMENT_3D('',#14835,#10636,#10637);
#8962=AXIS2_PLACEMENT_3D('',#14841,#10638,#10639);
#8963=AXIS2_PLACEMENT_3D('',#14842,#10640,#10641);
#8964=AXIS2_PLACEMENT_3D('',#14843,#10642,#10643);
#8965=AXIS2_PLACEMENT_3D('',#14849,#10644,#10645);
#8966=AXIS2_PLACEMENT_3D('',#14850,#10646,#10647);
#8967=AXIS2_PLACEMENT_3D('',#14856,#10648,#10649);
#8968=AXIS2_PLACEMENT_3D('',#14857,#10650,#10651);
#8969=AXIS2_PLACEMENT_3D('',#14871,#10652,#10653);
#8970=AXIS2_PLACEMENT_3D('',#14872,#10654,#10655);
#8971=AXIS2_PLACEMENT_3D('',#14874,#10656,#10657);
#8972=AXIS2_PLACEMENT_3D('',#14876,#10658,#10659);
#8973=AXIS2_PLACEMENT_3D('',#14888,#10660,#10661);
#8974=AXIS2_PLACEMENT_3D('',#14890,#10662,#10663);
#8975=AXIS2_PLACEMENT_3D('',#14896,#10664,#10665);
#8976=AXIS2_PLACEMENT_3D('',#14898,#10666,#10667);
#8977=AXIS2_PLACEMENT_3D('',#14900,#10668,#10669);
#8978=AXIS2_PLACEMENT_3D('',#14911,#10670,#10671);
#8979=AXIS2_PLACEMENT_3D('',#14913,#10672,#10673);
#8980=AXIS2_PLACEMENT_3D('',#14915,#10674,#10675);
#8981=AXIS2_PLACEMENT_3D('',#14926,#10676,#10677);
#8982=AXIS2_PLACEMENT_3D('',#14928,#10678,#10679);
#8983=AXIS2_PLACEMENT_3D('',#14930,#10680,#10681);
#8984=AXIS2_PLACEMENT_3D('',#14941,#10682,#10683);
#8985=AXIS2_PLACEMENT_3D('',#14943,#10684,#10685);
#8986=AXIS2_PLACEMENT_3D('',#14945,#10686,#10687);
#8987=AXIS2_PLACEMENT_3D('',#14951,#10688,#10689);
#8988=AXIS2_PLACEMENT_3D('',#14963,#10690,#10691);
#8989=AXIS2_PLACEMENT_3D('',#14965,#10692,#10693);
#8990=AXIS2_PLACEMENT_3D('',#14966,#10694,#10695);
#8991=AXIS2_PLACEMENT_3D('',#14968,#10696,#10697);
#8992=AXIS2_PLACEMENT_3D('',#14970,#10698,#10699);
#8993=AXIS2_PLACEMENT_3D('',#14972,#10700,#10701);
#8994=AXIS2_PLACEMENT_3D('',#14974,#10702,#10703);
#8995=AXIS2_PLACEMENT_3D('',#14976,#10704,#10705);
#8996=AXIS2_PLACEMENT_3D('',#14978,#10706,#10707);
#8997=AXIS2_PLACEMENT_3D('',#14980,#10708,#10709);
#8998=AXIS2_PLACEMENT_3D('',#14982,#10710,#10711);
#8999=AXIS2_PLACEMENT_3D('',#14984,#10712,#10713);
#9000=AXIS2_PLACEMENT_3D('',#14986,#10714,#10715);
#9001=AXIS2_PLACEMENT_3D('',#14988,#10716,#10717);
#9002=AXIS2_PLACEMENT_3D('',#14990,#10718,#10719);
#9003=AXIS2_PLACEMENT_3D('',#14992,#10720,#10721);
#9004=AXIS2_PLACEMENT_3D('',#14994,#10722,#10723);
#9005=AXIS2_PLACEMENT_3D('',#14996,#10724,#10725);
#9006=AXIS2_PLACEMENT_3D('',#14998,#10726,#10727);
#9007=AXIS2_PLACEMENT_3D('',#15000,#10728,#10729);
#9008=AXIS2_PLACEMENT_3D('',#15002,#10730,#10731);
#9009=AXIS2_PLACEMENT_3D('',#15007,#10732,#10733);
#9010=AXIS2_PLACEMENT_3D('',#15008,#10734,#10735);
#9011=AXIS2_PLACEMENT_3D('',#15009,#10736,#10737);
#9012=AXIS2_PLACEMENT_3D('',#15010,#10738,#10739);
#9013=AXIS2_PLACEMENT_3D('',#15011,#10740,#10741);
#9014=AXIS2_PLACEMENT_3D('',#15012,#10742,#10743);
#9015=AXIS2_PLACEMENT_3D('',#15013,#10744,#10745);
#9016=AXIS2_PLACEMENT_3D('',#15014,#10746,#10747);
#9017=AXIS2_PLACEMENT_3D('',#15015,#10748,#10749);
#9018=AXIS2_PLACEMENT_3D('',#15016,#10750,#10751);
#9019=AXIS2_PLACEMENT_3D('',#15017,#10752,#10753);
#9020=AXIS2_PLACEMENT_3D('',#15018,#10754,#10755);
#9021=AXIS2_PLACEMENT_3D('',#15019,#10756,#10757);
#9022=AXIS2_PLACEMENT_3D('',#15020,#10758,#10759);
#9023=AXIS2_PLACEMENT_3D('',#15021,#10760,#10761);
#9024=AXIS2_PLACEMENT_3D('',#15022,#10762,#10763);
#9025=AXIS2_PLACEMENT_3D('',#15023,#10764,#10765);
#9026=AXIS2_PLACEMENT_3D('',#15024,#10766,#10767);
#9027=AXIS2_PLACEMENT_3D('',#15025,#10768,#10769);
#9028=AXIS2_PLACEMENT_3D('',#15030,#10770,#10771);
#9029=AXIS2_PLACEMENT_3D('',#15035,#10772,#10773);
#9030=AXIS2_PLACEMENT_3D('',#15040,#10774,#10775);
#9031=AXIS2_PLACEMENT_3D('',#15045,#10776,#10777);
#9032=AXIS2_PLACEMENT_3D('',#15046,#10778,#10779);
#9033=AXIS2_PLACEMENT_3D('',#15051,#10780,#10781);
#9034=AXIS2_PLACEMENT_3D('',#15056,#10782,#10783);
#9035=AXIS2_PLACEMENT_3D('',#15061,#10784,#10785);
#9036=AXIS2_PLACEMENT_3D('',#15066,#10786,#10787);
#9037=AXIS2_PLACEMENT_3D('',#15067,#10788,#10789);
#9038=AXIS2_PLACEMENT_3D('',#15072,#10790,#10791);
#9039=AXIS2_PLACEMENT_3D('',#15077,#10792,#10793);
#9040=AXIS2_PLACEMENT_3D('',#15082,#10794,#10795);
#9041=AXIS2_PLACEMENT_3D('',#15083,#10796,#10797);
#9042=AXIS2_PLACEMENT_3D('',#15088,#10798,#10799);
#9043=AXIS2_PLACEMENT_3D('',#15093,#10800,#10801);
#9044=AXIS2_PLACEMENT_3D('',#15098,#10802,#10803);
#9045=AXIS2_PLACEMENT_3D('',#15103,#10804,#10805);
#9046=AXIS2_PLACEMENT_3D('',#15104,#10806,#10807);
#9047=AXIS2_PLACEMENT_3D('',#15109,#10808,#10809);
#9048=AXIS2_PLACEMENT_3D('',#15114,#10810,#10811);
#9049=AXIS2_PLACEMENT_3D('',#15119,#10812,#10813);
#9050=AXIS2_PLACEMENT_3D('',#15124,#10814,#10815);
#9051=AXIS2_PLACEMENT_3D('',#15125,#10816,#10817);
#9052=AXIS2_PLACEMENT_3D('',#15130,#10818,#10819);
#9053=AXIS2_PLACEMENT_3D('',#15135,#10820,#10821);
#9054=AXIS2_PLACEMENT_3D('',#15140,#10822,#10823);
#9055=AXIS2_PLACEMENT_3D('',#15145,#10824,#10825);
#9056=AXIS2_PLACEMENT_3D('',#15146,#10826,#10827);
#9057=AXIS2_PLACEMENT_3D('',#15147,#10828,#10829);
#9058=AXIS2_PLACEMENT_3D('',#15161,#10830,#10831);
#9059=AXIS2_PLACEMENT_3D('',#15162,#10832,#10833);
#9060=AXIS2_PLACEMENT_3D('',#15176,#10834,#10835);
#9061=AXIS2_PLACEMENT_3D('',#15177,#10836,#10837);
#9062=AXIS2_PLACEMENT_3D('',#15191,#10838,#10839);
#9063=AXIS2_PLACEMENT_3D('',#15192,#10840,#10841);
#9064=AXIS2_PLACEMENT_3D('',#15206,#10842,#10843);
#9065=AXIS2_PLACEMENT_3D('',#15207,#10844,#10845);
#9066=AXIS2_PLACEMENT_3D('',#15208,#10846,#10847);
#9067=AXIS2_PLACEMENT_3D('',#15210,#10848,#10849);
#9068=AXIS2_PLACEMENT_3D('',#15211,#10850,#10851);
#9069=AXIS2_PLACEMENT_3D('',#15225,#10852,#10853);
#9070=AXIS2_PLACEMENT_3D('',#15226,#10854,#10855);
#9071=AXIS2_PLACEMENT_3D('',#15234,#10856,#10857);
#9072=AXIS2_PLACEMENT_3D('',#15241,#10858,#10859);
#9073=AXIS2_PLACEMENT_3D('',#15248,#10860,#10861);
#9074=AXIS2_PLACEMENT_3D('',#15255,#10862,#10863);
#9075=AXIS2_PLACEMENT_3D('',#15262,#10864,#10865);
#9076=AXIS2_PLACEMENT_3D('',#15269,#10866,#10867);
#9077=AXIS2_PLACEMENT_3D('',#15276,#10868,#10869);
#9078=AXIS2_PLACEMENT_3D('',#15283,#10870,#10871);
#9079=AXIS2_PLACEMENT_3D('',#15290,#10872,#10873);
#9080=AXIS2_PLACEMENT_3D('',#15297,#10874,#10875);
#9081=AXIS2_PLACEMENT_3D('',#15304,#10876,#10877);
#9082=AXIS2_PLACEMENT_3D('',#15310,#10878,#10879);
#9083=AXIS2_PLACEMENT_3D('',#15312,#10880,#10881);
#9084=AXIS2_PLACEMENT_3D('',#15315,#10882,#10883);
#9085=AXIS2_PLACEMENT_3D('',#15316,#10884,#10885);
#9086=AXIS2_PLACEMENT_3D('',#15318,#10886,#10887);
#9087=AXIS2_PLACEMENT_3D('',#15320,#10888,#10889);
#9088=AXIS2_PLACEMENT_3D('',#15323,#10890,#10891);
#9089=AXIS2_PLACEMENT_3D('',#15324,#10892,#10893);
#9090=AXIS2_PLACEMENT_3D('',#15326,#10894,#10895);
#9091=AXIS2_PLACEMENT_3D('',#15327,#10896,#10897);
#9092=AXIS2_PLACEMENT_3D('',#15359,#10898,#10899);
#9093=AXIS2_PLACEMENT_3D('',#15391,#10900,#10901);
#9094=AXIS2_PLACEMENT_3D('',#15392,#10902,#10903);
#9095=AXIS2_PLACEMENT_3D('',#15457,#10904,#10905);
#9096=AXIS2_PLACEMENT_3D('',#15458,#10906,#10907);
#9097=AXIS2_PLACEMENT_3D('',#15466,#10908,#10909);
#9098=AXIS2_PLACEMENT_3D('',#15467,#10910,#10911);
#9099=AXIS2_PLACEMENT_3D('',#15478,#10912,#10913);
#9100=AXIS2_PLACEMENT_3D('',#15486,#10914,#10915);
#9101=AXIS2_PLACEMENT_3D('',#15493,#10916,#10917);
#9102=AXIS2_PLACEMENT_3D('',#15495,#10918,#10919);
#9103=AXIS2_PLACEMENT_3D('',#15496,#10920,#10921);
#9104=AXIS2_PLACEMENT_3D('',#15504,#10922,#10923);
#9105=AXIS2_PLACEMENT_3D('',#15506,#10924,#10925);
#9106=AXIS2_PLACEMENT_3D('',#15507,#10926,#10927);
#9107=AXIS2_PLACEMENT_3D('',#15508,#10928,#10929);
#9108=AXIS2_PLACEMENT_3D('',#15519,#10930,#10931);
#9109=AXIS2_PLACEMENT_3D('',#15520,#10932,#10933);
#9110=AXIS2_PLACEMENT_3D('',#15521,#10934,#10935);
#9111=AXIS2_PLACEMENT_3D('',#15529,#10936,#10937);
#9112=AXIS2_PLACEMENT_3D('',#15530,#10938,#10939);
#9113=AXIS2_PLACEMENT_3D('',#15549,#10940,#10941);
#9114=AXIS2_PLACEMENT_3D('',#15569,#10942,#10943);
#9115=AXIS2_PLACEMENT_3D('',#15583,#10944,#10945);
#9116=AXIS2_PLACEMENT_3D('',#15588,#10946,#10947);
#9117=AXIS2_PLACEMENT_3D('',#15603,#10948,#10949);
#9118=AXIS2_PLACEMENT_3D('',#15623,#10950,#10951);
#9119=AXIS2_PLACEMENT_3D('',#15637,#10952,#10953);
#9120=AXIS2_PLACEMENT_3D('',#15647,#10954,#10955);
#9121=AXIS2_PLACEMENT_3D('',#15653,#10956,#10957);
#9122=AXIS2_PLACEMENT_3D('',#15654,#10958,#10959);
#9123=AXIS2_PLACEMENT_3D('',#15655,#10960,#10961);
#9124=AXIS2_PLACEMENT_3D('',#15657,#10962,#10963);
#9125=AXIS2_PLACEMENT_3D('',#15668,#10964,#10965);
#9126=AXIS2_PLACEMENT_3D('',#15682,#10966,#10967);
#9127=AXIS2_PLACEMENT_3D('',#15687,#10968,#10969);
#9128=AXIS2_PLACEMENT_3D('',#15702,#10970,#10971);
#9129=AXIS2_PLACEMENT_3D('',#15722,#10972,#10973);
#9130=AXIS2_PLACEMENT_3D('',#15736,#10974,#10975);
#9131=AXIS2_PLACEMENT_3D('',#15741,#10976,#10977);
#9132=AXIS2_PLACEMENT_3D('',#15756,#10978,#10979);
#9133=AXIS2_PLACEMENT_3D('',#15776,#10980,#10981);
#9134=AXIS2_PLACEMENT_3D('',#15790,#10982,#10983);
#9135=AXIS2_PLACEMENT_3D('',#15795,#10984,#10985);
#9136=AXIS2_PLACEMENT_3D('',#15810,#10986,#10987);
#9137=AXIS2_PLACEMENT_3D('',#15830,#10988,#10989);
#9138=AXIS2_PLACEMENT_3D('',#15844,#10990,#10991);
#9139=AXIS2_PLACEMENT_3D('',#15845,#10992,#10993);
#9140=AXIS2_PLACEMENT_3D('',#15881,#10994,#10995);
#9141=AXIS2_PLACEMENT_3D('',#15887,#10996,#10997);
#9142=AXIS2_PLACEMENT_3D('',#15919,#10998,#10999);
#9143=AXIS2_PLACEMENT_3D('',#15924,#11000,#11001);
#9144=AXIS2_PLACEMENT_3D('',#15960,#11002,#11003);
#9145=AXIS2_PLACEMENT_3D('',#15996,#11004,#11005);
#9146=AXIS2_PLACEMENT_3D('',#16032,#11006,#11007);
#9147=AXIS2_PLACEMENT_3D('',#16068,#11008,#11009);
#9148=AXIS2_PLACEMENT_3D('',#16125,#11010,#11011);
#9149=AXIS2_PLACEMENT_3D('',#16182,#11012,#11013);
#9150=AXIS2_PLACEMENT_3D('',#16237,#11014,#11015);
#9151=AXIS2_PLACEMENT_3D('',#16294,#11016,#11017);
#9152=AXIS2_PLACEMENT_3D('',#16351,#11018,#11019);
#9153=AXIS2_PLACEMENT_3D('',#16406,#11020,#11021);
#9154=AXIS2_PLACEMENT_3D('',#16416,#11022,#11023);
#9155=AXIS2_PLACEMENT_3D('',#16426,#11024,#11025);
#9156=AXIS2_PLACEMENT_3D('',#16431,#11026,#11027);
#9157=AXIS2_PLACEMENT_3D('',#16441,#11028,#11029);
#9158=AXIS2_PLACEMENT_3D('',#16451,#11030,#11031);
#9159=AXIS2_PLACEMENT_3D('',#16456,#11032,#11033);
#9160=AXIS2_PLACEMENT_3D('',#16461,#11034,#11035);
#9161=AXIS2_PLACEMENT_3D('',#16471,#11036,#11037);
#9162=AXIS2_PLACEMENT_3D('',#16477,#11038,#11039);
#9163=AXIS2_PLACEMENT_3D('',#16478,#11040,#11041);
#9164=AXIS2_PLACEMENT_3D('',#16488,#11042,#11043);
#9165=AXIS2_PLACEMENT_3D('',#16498,#11044,#11045);
#9166=AXIS2_PLACEMENT_3D('',#16503,#11046,#11047);
#9167=AXIS2_PLACEMENT_3D('',#16513,#11048,#11049);
#9168=AXIS2_PLACEMENT_3D('',#16523,#11050,#11051);
#9169=AXIS2_PLACEMENT_3D('',#16528,#11052,#11053);
#9170=AXIS2_PLACEMENT_3D('',#16538,#11054,#11055);
#9171=AXIS2_PLACEMENT_3D('',#16548,#11056,#11057);
#9172=AXIS2_PLACEMENT_3D('',#16751,#11058,#11059);
#9173=AXIS2_PLACEMENT_3D('',#16752,#11060,#11061);
#9174=AXIS2_PLACEMENT_3D('',#16927,#11062,#11063);
#9175=AXIS2_PLACEMENT_3D('',#17126,#11064,#11065);
#9176=AXIS2_PLACEMENT_3D('',#17127,#11066,#11067);
#9177=AXIS2_PLACEMENT_3D('',#17302,#11068,#11069);
#9178=AXIS2_PLACEMENT_3D('',#17307,#11070,#11071);
#9179=AXIS2_PLACEMENT_3D('',#17506,#11072,#11073);
#9180=AXIS2_PLACEMENT_3D('',#17507,#11074,#11075);
#9181=AXIS2_PLACEMENT_3D('',#17682,#11076,#11077);
#9182=AXIS2_PLACEMENT_3D('',#17881,#11078,#11079);
#9183=AXIS2_PLACEMENT_3D('',#17882,#11080,#11081);
#9184=AXIS2_PLACEMENT_3D('',#18057,#11082,#11083);
#9185=AXIS2_PLACEMENT_3D('',#18256,#11084,#11085);
#9186=AXIS2_PLACEMENT_3D('',#18257,#11086,#11087);
#9187=AXIS2_PLACEMENT_3D('',#18432,#11088,#11089);
#9188=AXIS2_PLACEMENT_3D('',#18631,#11090,#11091);
#9189=AXIS2_PLACEMENT_3D('',#18632,#11092,#11093);
#9190=AXIS2_PLACEMENT_3D('',#18807,#11094,#11095);
#9191=AXIS2_PLACEMENT_3D('',#18808,#11096,#11097);
#9192=DIRECTION('',(0.,0.,1.));
#9193=DIRECTION('',(1.,0.,0.));
#9194=DIRECTION('',(1.,0.,0.));
#9195=DIRECTION('',(0.,0.,-1.));
#9196=DIRECTION('',(1.,0.,0.));
#9197=DIRECTION('',(0.,0.,-1.));
#9198=DIRECTION('',(1.,0.,0.));
#9199=DIRECTION('',(0.,0.,-1.));
#9200=DIRECTION('',(-1.,0.,0.));
#9201=DIRECTION('',(0.,0.,1.));
#9202=DIRECTION('',(-1.,0.,0.));
#9203=DIRECTION('',(0.,0.,1.));
#9204=DIRECTION('',(1.,-2.13742714109856E-17,-3.00478887951711E-17));
#9205=DIRECTION('',(-3.00478887951711E-17,0.,-1.));
#9206=DIRECTION('',(-1.,0.,0.));
#9207=DIRECTION('',(0.,0.,1.));
#9208=DIRECTION('',(-1.,0.,0.));
#9209=DIRECTION('',(0.,0.,1.));
#9210=DIRECTION('',(-1.,0.,0.));
#9211=DIRECTION('',(0.,0.,1.));
#9212=DIRECTION('',(-1.,0.,0.));
#9213=DIRECTION('',(0.,0.,1.));
#9214=DIRECTION('',(-1.,0.,0.));
#9215=DIRECTION('',(0.,0.,1.));
#9216=DIRECTION('',(-1.,0.,0.));
#9217=DIRECTION('',(0.,0.,1.));
#9218=DIRECTION('',(-1.,0.,0.));
#9219=DIRECTION('',(0.,0.,1.));
#9220=DIRECTION('',(-1.,0.,0.));
#9221=DIRECTION('',(0.,0.,1.));
#9222=DIRECTION('',(-1.,0.,0.));
#9223=DIRECTION('',(0.,0.,1.));
#9224=DIRECTION('',(-1.,0.,0.));
#9225=DIRECTION('',(0.,0.,1.));
#9226=DIRECTION('',(-1.,0.,0.));
#9227=DIRECTION('',(0.,0.,1.));
#9228=DIRECTION('',(-1.,0.,0.));
#9229=DIRECTION('',(0.,0.,1.));
#9230=DIRECTION('',(-1.,0.,0.));
#9231=DIRECTION('',(0.,0.,1.));
#9232=DIRECTION('',(-1.,0.,0.));
#9233=DIRECTION('',(0.,0.,1.));
#9234=DIRECTION('',(-1.,0.,0.));
#9235=DIRECTION('',(0.,0.,1.));
#9236=DIRECTION('',(-1.,0.,0.));
#9237=DIRECTION('',(0.,0.,1.));
#9238=DIRECTION('',(-1.,0.,0.));
#9239=DIRECTION('',(0.,0.,1.));
#9240=DIRECTION('',(-1.,0.,0.));
#9241=DIRECTION('',(0.,0.,1.));
#9242=DIRECTION('',(-1.,0.,0.));
#9243=DIRECTION('',(0.,0.,1.));
#9244=DIRECTION('',(-1.,0.,0.));
#9245=DIRECTION('',(0.,0.,1.));
#9246=DIRECTION('',(-1.,0.,0.));
#9247=DIRECTION('',(0.,0.,1.));
#9248=DIRECTION('',(-1.,0.,0.));
#9249=DIRECTION('',(0.,0.,1.));
#9250=DIRECTION('',(-1.,0.,0.));
#9251=DIRECTION('',(0.,0.,1.));
#9252=DIRECTION('',(-1.,0.,0.));
#9253=DIRECTION('',(0.,0.,1.));
#9254=DIRECTION('',(-1.,0.,0.));
#9255=DIRECTION('',(0.,0.,1.));
#9256=DIRECTION('',(-1.,0.,0.));
#9257=DIRECTION('',(0.,0.,1.));
#9258=DIRECTION('',(-1.,0.,0.));
#9259=DIRECTION('',(0.,0.,1.));
#9260=DIRECTION('',(-1.,0.,0.));
#9261=DIRECTION('',(0.,0.,1.));
#9262=DIRECTION('',(-1.,0.,0.));
#9263=DIRECTION('',(0.,0.,1.));
#9264=DIRECTION('',(-1.,0.,0.));
#9265=DIRECTION('',(0.,0.,1.));
#9266=DIRECTION('',(-1.,0.,0.));
#9267=DIRECTION('',(0.,0.,1.));
#9268=DIRECTION('',(-1.,0.,0.));
#9269=DIRECTION('',(0.,0.,1.));
#9270=DIRECTION('',(-1.,0.,0.));
#9271=DIRECTION('',(0.,0.,1.));
#9272=DIRECTION('',(-1.,0.,0.));
#9273=DIRECTION('',(0.,0.,1.));
#9274=DIRECTION('',(-1.,0.,0.));
#9275=DIRECTION('',(0.,0.,1.));
#9276=DIRECTION('',(-1.,0.,0.));
#9277=DIRECTION('',(0.,0.,1.));
#9278=DIRECTION('',(-1.,0.,0.));
#9279=DIRECTION('',(0.,0.,1.));
#9280=DIRECTION('',(-1.,0.,0.));
#9281=DIRECTION('',(0.,0.,1.));
#9282=DIRECTION('',(-1.,0.,0.));
#9283=DIRECTION('',(0.,0.,1.));
#9284=DIRECTION('',(-1.,0.,0.));
#9285=DIRECTION('',(0.,0.,1.));
#9286=DIRECTION('',(-1.,0.,0.));
#9287=DIRECTION('',(0.,0.,1.));
#9288=DIRECTION('',(-1.,0.,0.));
#9289=DIRECTION('',(0.,0.,1.));
#9290=DIRECTION('',(-1.,0.,0.));
#9291=DIRECTION('',(0.,0.,1.));
#9292=DIRECTION('',(-1.,0.,0.));
#9293=DIRECTION('',(0.,0.,1.));
#9294=DIRECTION('',(1.,0.,0.));
#9295=DIRECTION('',(0.,0.,-1.));
#9296=DIRECTION('',(1.,0.,0.));
#9297=DIRECTION('',(0.,0.,-1.));
#9298=DIRECTION('',(0.,0.,1.));
#9299=DIRECTION('',(1.,0.,0.));
#9300=DIRECTION('',(-1.,0.,0.));
#9301=DIRECTION('',(0.,0.,1.));
#9302=DIRECTION('',(-1.,0.,0.));
#9303=DIRECTION('',(0.,0.,1.));
#9304=DIRECTION('',(1.76366925757084E-19,0.309016994741914,-0.951056516175919));
#9305=DIRECTION('',(0.,0.951056516175919,0.309016994741914));
#9306=DIRECTION('',(1.,5.11915082809089E-15,2.61659684133968E-15));
#9307=DIRECTION('',(-5.11915082809089E-15,1.,0.));
#9308=DIRECTION('',(1.,0.,0.));
#9309=DIRECTION('',(0.,0.,-1.));
#9310=DIRECTION('',(4.91605234155644E-18,-0.30901699293847,0.951056516761893));
#9311=DIRECTION('',(0.,-0.951056516761893,-0.30901699293847));
#9312=DIRECTION('',(-1.,0.,0.));
#9313=DIRECTION('',(0.,0.,1.));
#9314=DIRECTION('',(-1.,0.,0.));
#9315=DIRECTION('',(0.,0.,1.));
#9316=DIRECTION('',(2.10154074524954E-18,0.587785252825749,-0.8090169939875));
#9317=DIRECTION('',(0.,0.8090169939875,0.587785252825749));
#9318=DIRECTION('',(1.,3.54488757105866E-15,2.81393787529885E-15));
#9319=DIRECTION('',(-3.54488757105866E-15,1.,0.));
#9320=DIRECTION('',(1.,0.,0.));
#9321=DIRECTION('',(0.,0.,-1.));
#9322=DIRECTION('',(2.58121594927379E-20,-0.58778525152076,0.80901699493563));
#9323=DIRECTION('',(0.,-0.80901699493563,-0.58778525152076));
#9324=DIRECTION('',(-1.,0.,0.));
#9325=DIRECTION('',(0.,0.,1.));
#9326=DIRECTION('',(-1.,0.,0.));
#9327=DIRECTION('',(0.,0.,1.));
#9328=DIRECTION('',(-9.01993783845845E-19,0.809016994935629,-0.587785251520761));
#9329=DIRECTION('',(0.,0.587785251520761,0.809016994935629));
#9330=DIRECTION('',(1.,2.93053751101568E-15,3.40384429899751E-15));
#9331=DIRECTION('',(3.40384429899751E-15,0.,-1.));
#9332=DIRECTION('',(1.,0.,0.));
#9333=DIRECTION('',(0.,0.,-1.));
#9334=DIRECTION('',(4.61321756981649E-18,-0.8090169939875,0.587785252825748));
#9335=DIRECTION('',(0.,-0.587785252825748,-0.8090169939875));
#9336=DIRECTION('',(-1.,0.,0.));
#9337=DIRECTION('',(0.,0.,1.));
#9338=DIRECTION('',(-1.,0.,0.));
#9339=DIRECTION('',(0.,0.,1.));
#9340=DIRECTION('',(5.97474930064793E-18,0.951056516761894,-0.30901699293847));
#9341=DIRECTION('',(0.,0.30901699293847,0.951056516761894));
#9342=DIRECTION('',(1.,2.72501936239058E-15,4.91547108693002E-15));
#9343=DIRECTION('',(4.91547108693002E-15,0.,-1.));
#9344=DIRECTION('',(1.,0.,0.));
#9345=DIRECTION('',(0.,0.,-1.));
#9346=DIRECTION('',(-1.90367459747866E-18,-0.951056516175919,0.309016994741914));
#9347=DIRECTION('',(0.,-0.309016994741914,-0.951056516175919));
#9348=DIRECTION('',(-1.,0.,0.));
#9349=DIRECTION('',(0.,0.,1.));
#9350=DIRECTION('',(-1.,0.,0.));
#9351=DIRECTION('',(0.,0.,1.));
#9352=DIRECTION('',(0.,1.,0.));
#9353=DIRECTION('',(0.,0.,1.));
#9354=DIRECTION('',(1.,0.,0.));
#9355=DIRECTION('',(0.,0.,-1.));
#9356=DIRECTION('',(1.,0.,0.));
#9357=DIRECTION('',(0.,0.,-1.));
#9358=DIRECTION('',(0.,-1.,0.));
#9359=DIRECTION('',(0.,0.,-1.));
#9360=DIRECTION('',(-1.,0.,0.));
#9361=DIRECTION('',(0.,0.,1.));
#9362=DIRECTION('',(-1.,0.,0.));
#9363=DIRECTION('',(0.,0.,1.));
#9364=DIRECTION('',(1.76366925757084E-19,0.951056516175919,0.309016994741914));
#9365=DIRECTION('',(0.,-0.309016994741914,0.951056516175919));
#9366=DIRECTION('',(1.,2.72501936239123E-15,4.91547108693002E-15));
#9367=DIRECTION('',(4.91547108693002E-15,0.,-1.));
#9368=DIRECTION('',(1.,0.,0.));
#9369=DIRECTION('',(0.,0.,-1.));
#9370=DIRECTION('',(4.91605234155644E-18,-0.951056516761893,-0.30901699293847));
#9371=DIRECTION('',(0.,0.30901699293847,-0.951056516761893));
#9372=DIRECTION('',(-1.,0.,0.));
#9373=DIRECTION('',(0.,0.,1.));
#9374=DIRECTION('',(-1.,0.,0.));
#9375=DIRECTION('',(0.,0.,1.));
#9376=DIRECTION('',(2.10154074524954E-18,0.8090169939875,0.587785252825749));
#9377=DIRECTION('',(0.,-0.587785252825749,0.8090169939875));
#9378=DIRECTION('',(1.,2.93053751101741E-15,3.40384429899751E-15));
#9379=DIRECTION('',(3.40384429899751E-15,0.,-1.));
#9380=DIRECTION('',(1.,0.,0.));
#9381=DIRECTION('',(0.,0.,-1.));
#9382=DIRECTION('',(2.58121594927379E-20,-0.80901699493563,-0.58778525152076));
#9383=DIRECTION('',(0.,0.58778525152076,-0.80901699493563));
#9384=DIRECTION('',(-1.,0.,0.));
#9385=DIRECTION('',(0.,0.,1.));
#9386=DIRECTION('',(-1.,0.,0.));
#9387=DIRECTION('',(0.,0.,1.));
#9388=DIRECTION('',(-9.01993783845845E-19,0.587785251520761,0.809016994935629));
#9389=DIRECTION('',(0.,-0.809016994935629,0.587785251520761));
#9390=DIRECTION('',(1.,3.54488757106004E-15,2.81393787529885E-15));
#9391=DIRECTION('',(-3.54488757106004E-15,1.,0.));
#9392=DIRECTION('',(1.,0.,0.));
#9393=DIRECTION('',(0.,0.,-1.));
#9394=DIRECTION('',(4.61321756981649E-18,-0.587785252825748,-0.8090169939875));
#9395=DIRECTION('',(0.,0.8090169939875,-0.587785252825748));
#9396=DIRECTION('',(-1.,0.,0.));
#9397=DIRECTION('',(0.,0.,1.));
#9398=DIRECTION('',(-1.,0.,0.));
#9399=DIRECTION('',(0.,0.,1.));
#9400=DIRECTION('',(5.97474930064793E-18,0.30901699293847,0.951056516761894));
#9401=DIRECTION('',(0.,-0.951056516761894,0.30901699293847));
#9402=DIRECTION('',(1.,5.11915082809161E-15,2.61659684133968E-15));
#9403=DIRECTION('',(-5.11915082809161E-15,1.,0.));
#9404=DIRECTION('',(1.,0.,0.));
#9405=DIRECTION('',(0.,0.,-1.));
#9406=DIRECTION('',(-1.90367459747866E-18,-0.309016994741914,-0.951056516175919));
#9407=DIRECTION('',(0.,0.951056516175919,-0.309016994741914));
#9408=DIRECTION('',(-1.,0.,0.));
#9409=DIRECTION('',(0.,0.,1.));
#9410=DIRECTION('',(-1.,0.,0.));
#9411=DIRECTION('',(0.,0.,1.));
#9412=DIRECTION('',(0.,0.,1.));
#9413=DIRECTION('',(1.,0.,0.));
#9414=DIRECTION('',(1.,0.,0.));
#9415=DIRECTION('',(0.,0.,-1.));
#9416=DIRECTION('',(1.,0.,0.));
#9417=DIRECTION('',(0.,0.,-1.));
#9418=DIRECTION('',(0.,0.,-1.));
#9419=DIRECTION('',(-1.,0.,0.));
#9420=DIRECTION('',(-1.,0.,0.));
#9421=DIRECTION('',(0.,0.,1.));
#9422=DIRECTION('',(-1.,0.,0.));
#9423=DIRECTION('',(0.,0.,1.));
#9424=DIRECTION('',(1.76366925757084E-19,-0.309016994741914,0.951056516175919));
#9425=DIRECTION('',(0.,-0.951056516175919,-0.309016994741914));
#9426=DIRECTION('',(1.,5.11915082809161E-15,2.61659684133999E-15));
#9427=DIRECTION('',(-5.11915082809161E-15,1.,0.));
#9428=DIRECTION('',(1.,0.,0.));
#9429=DIRECTION('',(0.,0.,-1.));
#9430=DIRECTION('',(4.91605234155644E-18,0.30901699293847,-0.951056516761893));
#9431=DIRECTION('',(0.,0.951056516761893,0.30901699293847));
#9432=DIRECTION('',(-1.,0.,0.));
#9433=DIRECTION('',(0.,0.,1.));
#9434=DIRECTION('',(-1.,0.,0.));
#9435=DIRECTION('',(0.,0.,1.));
#9436=DIRECTION('',(2.10154074524954E-18,-0.587785252825749,0.8090169939875));
#9437=DIRECTION('',(0.,-0.8090169939875,-0.587785252825749));
#9438=DIRECTION('',(1.,3.54488757106004E-15,2.81393787529969E-15));
#9439=DIRECTION('',(-3.54488757106004E-15,1.,0.));
#9440=DIRECTION('',(1.,0.,0.));
#9441=DIRECTION('',(0.,0.,-1.));
#9442=DIRECTION('',(2.58121594927379E-20,0.58778525152076,-0.80901699493563));
#9443=DIRECTION('',(0.,0.80901699493563,0.58778525152076));
#9444=DIRECTION('',(-1.,0.,0.));
#9445=DIRECTION('',(0.,0.,1.));
#9446=DIRECTION('',(-1.,0.,0.));
#9447=DIRECTION('',(0.,0.,1.));
#9448=DIRECTION('',(-9.01993783845845E-19,-0.809016994935629,0.587785251520761));
#9449=DIRECTION('',(0.,-0.587785251520761,-0.809016994935629));
#9450=DIRECTION('',(1.,2.93053751101741E-15,3.4038442990036E-15));
#9451=DIRECTION('',(3.4038442990036E-15,0.,-1.));
#9452=DIRECTION('',(1.,0.,0.));
#9453=DIRECTION('',(0.,0.,-1.));
#9454=DIRECTION('',(4.61321756981649E-18,0.8090169939875,-0.587785252825748));
#9455=DIRECTION('',(0.,0.587785252825748,0.8090169939875));
#9456=DIRECTION('',(-1.,0.,0.));
#9457=DIRECTION('',(0.,0.,1.));
#9458=DIRECTION('',(-1.,0.,0.));
#9459=DIRECTION('',(0.,0.,1.));
#9460=DIRECTION('',(5.97474930064793E-18,-0.951056516761894,0.30901699293847));
#9461=DIRECTION('',(0.,-0.30901699293847,-0.951056516761894));
#9462=DIRECTION('',(1.,2.72501936239123E-15,4.91547108691513E-15));
#9463=DIRECTION('',(4.91547108691513E-15,0.,-1.));
#9464=DIRECTION('',(1.,0.,0.));
#9465=DIRECTION('',(0.,0.,-1.));
#9466=DIRECTION('',(-1.90367459747866E-18,0.951056516175919,-0.309016994741914));
#9467=DIRECTION('',(0.,0.309016994741914,0.951056516175919));
#9468=DIRECTION('',(-1.,0.,0.));
#9469=DIRECTION('',(0.,0.,1.));
#9470=DIRECTION('',(-1.,0.,0.));
#9471=DIRECTION('',(0.,0.,1.));
#9472=DIRECTION('',(0.,-1.,0.));
#9473=DIRECTION('',(0.,0.,-1.));
#9474=DIRECTION('',(1.,0.,0.));
#9475=DIRECTION('',(0.,0.,-1.));
#9476=DIRECTION('',(1.,0.,0.));
#9477=DIRECTION('',(0.,0.,-1.));
#9478=DIRECTION('',(0.,1.,0.));
#9479=DIRECTION('',(0.,0.,1.));
#9480=DIRECTION('',(-1.,0.,0.));
#9481=DIRECTION('',(0.,0.,1.));
#9482=DIRECTION('',(-1.,0.,0.));
#9483=DIRECTION('',(0.,0.,1.));
#9484=DIRECTION('',(1.76366925757084E-19,-0.951056516175919,-0.309016994741914));
#9485=DIRECTION('',(0.,0.309016994741914,-0.951056516175919));
#9486=DIRECTION('',(1.,2.72501936239058E-15,4.91547108691514E-15));
#9487=DIRECTION('',(4.91547108691514E-15,0.,-1.));
#9488=DIRECTION('',(1.,0.,0.));
#9489=DIRECTION('',(0.,0.,-1.));
#9490=DIRECTION('',(4.91605234155644E-18,0.951056516761893,0.30901699293847));
#9491=DIRECTION('',(0.,-0.30901699293847,0.951056516761893));
#9492=DIRECTION('',(-1.,0.,0.));
#9493=DIRECTION('',(0.,0.,1.));
#9494=DIRECTION('',(-1.,0.,0.));
#9495=DIRECTION('',(0.,0.,1.));
#9496=DIRECTION('',(2.10154074524954E-18,-0.8090169939875,-0.587785252825749));
#9497=DIRECTION('',(0.,0.587785252825749,-0.8090169939875));
#9498=DIRECTION('',(1.,2.93053751101568E-15,3.4038442990036E-15));
#9499=DIRECTION('',(3.4038442990036E-15,0.,-1.));
#9500=DIRECTION('',(1.,0.,0.));
#9501=DIRECTION('',(0.,0.,-1.));
#9502=DIRECTION('',(2.58121594927379E-20,0.80901699493563,0.58778525152076));
#9503=DIRECTION('',(0.,-0.58778525152076,0.80901699493563));
#9504=DIRECTION('',(-1.,0.,0.));
#9505=DIRECTION('',(0.,0.,1.));
#9506=DIRECTION('',(-1.,0.,0.));
#9507=DIRECTION('',(0.,0.,1.));
#9508=DIRECTION('',(-9.01993783845845E-19,-0.587785251520761,-0.809016994935629));
#9509=DIRECTION('',(0.,0.809016994935629,-0.587785251520761));
#9510=DIRECTION('',(1.,3.54488757105866E-15,2.81393787529969E-15));
#9511=DIRECTION('',(-3.54488757105866E-15,1.,0.));
#9512=DIRECTION('',(1.,0.,0.));
#9513=DIRECTION('',(0.,0.,-1.));
#9514=DIRECTION('',(4.61321756981649E-18,0.587785252825748,0.8090169939875));
#9515=DIRECTION('',(0.,-0.8090169939875,0.587785252825748));
#9516=DIRECTION('',(-1.,0.,0.));
#9517=DIRECTION('',(0.,0.,1.));
#9518=DIRECTION('',(-1.,0.,0.));
#9519=DIRECTION('',(0.,0.,1.));
#9520=DIRECTION('',(5.97474930064793E-18,-0.30901699293847,-0.951056516761894));
#9521=DIRECTION('',(0.,0.951056516761894,-0.30901699293847));
#9522=DIRECTION('',(1.,5.11915082809089E-15,2.61659684133999E-15));
#9523=DIRECTION('',(-5.11915082809089E-15,1.,0.));
#9524=DIRECTION('',(1.,0.,0.));
#9525=DIRECTION('',(0.,0.,-1.));
#9526=DIRECTION('',(-1.90367459747866E-18,0.309016994741914,0.951056516175919));
#9527=DIRECTION('',(0.,-0.951056516175919,0.309016994741914));
#9528=DIRECTION('',(-1.,0.,0.));
#9529=DIRECTION('',(0.,0.,1.));
#9530=DIRECTION('',(-1.,0.,0.));
#9531=DIRECTION('',(0.,0.,1.));
#9532=DIRECTION('',(0.,0.,-1.));
#9533=DIRECTION('',(-1.,0.,0.));
#9534=DIRECTION('',(1.,0.,0.));
#9535=DIRECTION('',(0.,0.,-1.));
#9536=DIRECTION('',(-1.,0.,0.));
#9537=DIRECTION('',(0.,0.,1.));
#9538=DIRECTION('',(1.,0.,0.));
#9539=DIRECTION('',(0.,0.,-1.));
#9540=DIRECTION('',(1.,0.,0.));
#9541=DIRECTION('',(0.,0.,-1.));
#9542=DIRECTION('',(-2.99135772045791E-17,-0.130526192305464,-0.991444861362566));
#9543=DIRECTION('',(0.,0.991444861362566,-0.130526192305464));
#9544=DIRECTION('',(3.22859531325E-17,-0.430511096755578,0.902585284375005));
#9545=DIRECTION('',(0.,-0.902585284375005,-0.430511096755578));
#9546=DIRECTION('',(-1.,0.,0.));
#9547=DIRECTION('',(0.,0.,1.));
#9548=DIRECTION('',(-1.,0.,0.));
#9549=DIRECTION('',(0.,0.,1.));
#9550=DIRECTION('',(-1.,0.,0.));
#9551=DIRECTION('',(0.,0.,1.));
#9552=DIRECTION('',(-1.,0.,0.));
#9553=DIRECTION('',(0.,0.,1.));
#9554=DIRECTION('',(-1.,0.,0.));
#9555=DIRECTION('',(0.,0.,1.));
#9556=DIRECTION('',(-1.,0.,0.));
#9557=DIRECTION('',(0.,0.,1.));
#9558=DIRECTION('',(-1.,0.,0.));
#9559=DIRECTION('',(0.,0.,1.));
#9560=DIRECTION('',(-1.,0.,0.));
#9561=DIRECTION('',(0.,0.,1.));
#9562=DIRECTION('',(-1.,0.,0.));
#9563=DIRECTION('',(0.,0.,1.));
#9564=DIRECTION('',(-1.,0.,0.));
#9565=DIRECTION('',(0.,0.,1.));
#9566=DIRECTION('',(-1.,0.,0.));
#9567=DIRECTION('',(0.,0.,1.));
#9568=DIRECTION('',(-1.,0.,0.));
#9569=DIRECTION('',(0.,0.,1.));
#9570=DIRECTION('',(-1.,0.,0.));
#9571=DIRECTION('',(0.,0.,1.));
#9572=DIRECTION('',(-1.,0.,0.));
#9573=DIRECTION('',(0.,0.,1.));
#9574=DIRECTION('',(-1.,0.,0.));
#9575=DIRECTION('',(0.,0.,1.));
#9576=DIRECTION('',(-1.,0.,0.));
#9577=DIRECTION('',(0.,0.,1.));
#9578=DIRECTION('',(-1.,0.,0.));
#9579=DIRECTION('',(0.,0.,1.));
#9580=DIRECTION('',(-1.,0.,0.));
#9581=DIRECTION('',(0.,0.,1.));
#9582=DIRECTION('',(-1.,0.,0.));
#9583=DIRECTION('',(0.,0.,1.));
#9584=DIRECTION('',(-1.,0.,0.));
#9585=DIRECTION('',(0.,0.,1.));
#9586=DIRECTION('',(-1.,0.,0.));
#9587=DIRECTION('',(0.,0.,1.));
#9588=DIRECTION('',(-1.,0.,0.));
#9589=DIRECTION('',(0.,0.,1.));
#9590=DIRECTION('',(1.,0.,0.));
#9591=DIRECTION('',(0.,0.,-1.));
#9592=DIRECTION('',(1.,0.,0.));
#9593=DIRECTION('',(0.,0.,-1.));
#9594=DIRECTION('',(-6.60825936598169E-17,0.182235525591703,-0.983254907545503));
#9595=DIRECTION('',(0.,0.983254907545503,0.182235525591703));
#9596=DIRECTION('',(2.18592128542802E-17,-0.688354575657138,0.725374371047035));
#9597=DIRECTION('',(0.,-0.725374371047035,-0.688354575657138));
#9598=DIRECTION('',(1.,0.,0.));
#9599=DIRECTION('',(0.,0.,-1.));
#9600=DIRECTION('',(1.,0.,0.));
#9601=DIRECTION('',(0.,0.,-1.));
#9602=DIRECTION('',(8.04110715575716E-17,0.477158760378666,-0.878817112597322));
#9603=DIRECTION('',(0.,0.878817112597322,0.477158760378666));
#9604=DIRECTION('',(7.14896713846317E-17,-0.878817112597323,0.477158760378665));
#9605=DIRECTION('',(0.,-0.477158760378665,-0.878817112597323));
#9606=DIRECTION('',(1.,0.,0.));
#9607=DIRECTION('',(0.,0.,-1.));
#9608=DIRECTION('',(1.,0.,0.));
#9609=DIRECTION('',(0.,0.,-1.));
#9610=DIRECTION('',(1.8186512468286E-16,0.725374371047035,-0.688354575657138));
#9611=DIRECTION('',(0.,0.688354575657138,0.725374371047035));
#9612=DIRECTION('',(-4.64133914967143E-17,-0.983254907545503,0.182235525591703));
#9613=DIRECTION('',(0.,-0.182235525591703,-0.983254907545503));
#9614=DIRECTION('',(1.,0.,0.));
#9615=DIRECTION('',(0.,0.,-1.));
#9616=DIRECTION('',(1.,0.,0.));
#9617=DIRECTION('',(0.,0.,-1.));
#9618=DIRECTION('',(6.48328605787293E-17,0.902585284375005,-0.430511096755578));
#9619=DIRECTION('',(0.,0.430511096755578,0.902585284375005));
#9620=DIRECTION('',(-2.54736739925667E-17,-0.991444861362566,-0.130526192305464));
#9621=DIRECTION('',(0.,0.130526192305464,-0.991444861362566));
#9622=DIRECTION('',(1.,0.,0.));
#9623=DIRECTION('',(0.,0.,-1.));
#9624=DIRECTION('',(1.,0.,0.));
#9625=DIRECTION('',(0.,0.,-1.));
#9626=DIRECTION('',(-2.99135772045791E-17,0.991444861362566,-0.130526192305464));
#9627=DIRECTION('',(0.,0.130526192305464,0.991444861362566));
#9628=DIRECTION('',(3.22859531325E-17,-0.902585284375005,-0.430511096755578));
#9629=DIRECTION('',(0.,0.430511096755578,-0.902585284375005));
#9630=DIRECTION('',(1.,0.,0.));
#9631=DIRECTION('',(0.,0.,-1.));
#9632=DIRECTION('',(1.,0.,0.));
#9633=DIRECTION('',(0.,0.,-1.));
#9634=DIRECTION('',(-6.60825936598169E-17,0.983254907545503,0.182235525591703));
#9635=DIRECTION('',(0.,-0.182235525591703,0.983254907545503));
#9636=DIRECTION('',(2.18592128542802E-17,-0.725374371047035,-0.688354575657138));
#9637=DIRECTION('',(0.,0.688354575657138,-0.725374371047035));
#9638=DIRECTION('',(1.,0.,0.));
#9639=DIRECTION('',(0.,0.,-1.));
#9640=DIRECTION('',(1.,0.,0.));
#9641=DIRECTION('',(0.,0.,-1.));
#9642=DIRECTION('',(8.04110715575716E-17,0.878817112597322,0.477158760378666));
#9643=DIRECTION('',(0.,-0.477158760378666,0.878817112597322));
#9644=DIRECTION('',(7.14896713846317E-17,-0.477158760378665,-0.878817112597323));
#9645=DIRECTION('',(0.,0.878817112597323,-0.477158760378665));
#9646=DIRECTION('',(1.,0.,0.));
#9647=DIRECTION('',(0.,0.,-1.));
#9648=DIRECTION('',(1.,0.,0.));
#9649=DIRECTION('',(0.,0.,-1.));
#9650=DIRECTION('',(1.8186512468286E-16,0.688354575657138,0.725374371047035));
#9651=DIRECTION('',(0.,-0.725374371047035,0.688354575657138));
#9652=DIRECTION('',(-4.64133914967143E-17,-0.182235525591703,-0.983254907545503));
#9653=DIRECTION('',(0.,0.983254907545503,-0.182235525591703));
#9654=DIRECTION('',(1.,0.,0.));
#9655=DIRECTION('',(0.,0.,-1.));
#9656=DIRECTION('',(1.,0.,0.));
#9657=DIRECTION('',(0.,0.,-1.));
#9658=DIRECTION('',(6.48328605787293E-17,0.430511096755578,0.902585284375005));
#9659=DIRECTION('',(0.,-0.902585284375005,0.430511096755578));
#9660=DIRECTION('',(-2.54736739925667E-17,0.130526192305464,-0.991444861362566));
#9661=DIRECTION('',(0.,0.991444861362566,0.130526192305464));
#9662=DIRECTION('',(1.,0.,0.));
#9663=DIRECTION('',(0.,0.,-1.));
#9664=DIRECTION('',(1.,0.,0.));
#9665=DIRECTION('',(0.,0.,-1.));
#9666=DIRECTION('',(-2.99135772045791E-17,0.130526192305464,0.991444861362566));
#9667=DIRECTION('',(0.,-0.991444861362566,0.130526192305464));
#9668=DIRECTION('',(3.22859531325E-17,0.430511096755578,-0.902585284375005));
#9669=DIRECTION('',(0.,0.902585284375005,0.430511096755578));
#9670=DIRECTION('',(1.,0.,0.));
#9671=DIRECTION('',(0.,0.,-1.));
#9672=DIRECTION('',(1.,0.,0.));
#9673=DIRECTION('',(0.,0.,-1.));
#9674=DIRECTION('',(-6.60825936598169E-17,-0.182235525591703,0.983254907545503));
#9675=DIRECTION('',(0.,-0.983254907545503,-0.182235525591703));
#9676=DIRECTION('',(2.18592128542802E-17,0.688354575657138,-0.725374371047035));
#9677=DIRECTION('',(0.,0.725374371047035,0.688354575657138));
#9678=DIRECTION('',(1.,0.,0.));
#9679=DIRECTION('',(0.,0.,-1.));
#9680=DIRECTION('',(1.,0.,0.));
#9681=DIRECTION('',(0.,0.,-1.));
#9682=DIRECTION('',(8.04110715575716E-17,-0.477158760378666,0.878817112597322));
#9683=DIRECTION('',(0.,-0.878817112597322,-0.477158760378666));
#9684=DIRECTION('',(7.14896713846317E-17,0.878817112597323,-0.477158760378665));
#9685=DIRECTION('',(0.,0.477158760378665,0.878817112597323));
#9686=DIRECTION('',(1.,0.,0.));
#9687=DIRECTION('',(0.,0.,-1.));
#9688=DIRECTION('',(1.,0.,0.));
#9689=DIRECTION('',(0.,0.,-1.));
#9690=DIRECTION('',(1.8186512468286E-16,-0.725374371047035,0.688354575657138));
#9691=DIRECTION('',(0.,-0.688354575657138,-0.725374371047035));
#9692=DIRECTION('',(-4.64133914967143E-17,0.983254907545503,-0.182235525591703));
#9693=DIRECTION('',(0.,0.182235525591703,0.983254907545503));
#9694=DIRECTION('',(1.,0.,0.));
#9695=DIRECTION('',(0.,0.,-1.));
#9696=DIRECTION('',(1.,0.,0.));
#9697=DIRECTION('',(0.,0.,-1.));
#9698=DIRECTION('',(6.48328605787293E-17,-0.902585284375005,0.430511096755578));
#9699=DIRECTION('',(0.,-0.430511096755578,-0.902585284375005));
#9700=DIRECTION('',(-2.54736739925667E-17,0.991444861362566,0.130526192305464));
#9701=DIRECTION('',(0.,-0.130526192305464,0.991444861362566));
#9702=DIRECTION('',(1.,0.,0.));
#9703=DIRECTION('',(0.,0.,-1.));
#9704=DIRECTION('',(1.,0.,0.));
#9705=DIRECTION('',(0.,0.,-1.));
#9706=DIRECTION('',(-2.99135772045791E-17,-0.991444861362566,0.130526192305464));
#9707=DIRECTION('',(0.,-0.130526192305464,-0.991444861362566));
#9708=DIRECTION('',(3.22859531325E-17,0.902585284375005,0.430511096755578));
#9709=DIRECTION('',(0.,-0.430511096755578,0.902585284375005));
#9710=DIRECTION('',(1.,0.,0.));
#9711=DIRECTION('',(0.,0.,-1.));
#9712=DIRECTION('',(1.,0.,0.));
#9713=DIRECTION('',(0.,0.,-1.));
#9714=DIRECTION('',(-6.60825936598169E-17,-0.983254907545503,-0.182235525591703));
#9715=DIRECTION('',(0.,0.182235525591703,-0.983254907545503));
#9716=DIRECTION('',(2.18592128542802E-17,0.725374371047035,0.688354575657138));
#9717=DIRECTION('',(0.,-0.688354575657138,0.725374371047035));
#9718=DIRECTION('',(1.,0.,0.));
#9719=DIRECTION('',(0.,0.,-1.));
#9720=DIRECTION('',(1.,0.,0.));
#9721=DIRECTION('',(0.,0.,-1.));
#9722=DIRECTION('',(8.04110715575716E-17,-0.878817112597322,-0.477158760378666));
#9723=DIRECTION('',(0.,0.477158760378666,-0.878817112597322));
#9724=DIRECTION('',(7.14896713846317E-17,0.477158760378665,0.878817112597323));
#9725=DIRECTION('',(0.,-0.878817112597323,0.477158760378665));
#9726=DIRECTION('',(1.,0.,0.));
#9727=DIRECTION('',(0.,0.,-1.));
#9728=DIRECTION('',(1.,0.,0.));
#9729=DIRECTION('',(0.,0.,-1.));
#9730=DIRECTION('',(1.8186512468286E-16,-0.688354575657138,-0.725374371047035));
#9731=DIRECTION('',(0.,0.725374371047035,-0.688354575657138));
#9732=DIRECTION('',(-4.64133914967143E-17,0.182235525591703,0.983254907545503));
#9733=DIRECTION('',(0.,-0.983254907545503,0.182235525591703));
#9734=DIRECTION('',(1.,0.,0.));
#9735=DIRECTION('',(0.,0.,-1.));
#9736=DIRECTION('',(1.,0.,0.));
#9737=DIRECTION('',(0.,0.,-1.));
#9738=DIRECTION('',(6.48328605787293E-17,-0.430511096755578,-0.902585284375005));
#9739=DIRECTION('',(0.,0.902585284375005,-0.430511096755578));
#9740=DIRECTION('',(-2.54736739925667E-17,-0.130526192305464,0.991444861362566));
#9741=DIRECTION('',(0.,-0.991444861362566,-0.130526192305464));
#9742=DIRECTION('',(-1.,0.,0.));
#9743=DIRECTION('',(0.,0.,1.));
#9744=DIRECTION('',(-1.,0.,0.));
#9745=DIRECTION('',(0.,0.,1.));
#9746=DIRECTION('',(1.,-1.23512438660743E-15,-2.69129956548782E-15));
#9747=DIRECTION('',(-2.69129956548782E-15,0.,-1.));
#9748=DIRECTION('',(1.,-1.18123916154446E-15,-1.96770129996799E-15));
#9749=DIRECTION('',(-1.96770129996799E-15,0.,-1.));
#9750=DIRECTION('',(1.,-1.32688644717816E-16,-1.05641119487183E-16));
#9751=DIRECTION('',(1.32688644717816E-16,1.,0.));
#9752=DIRECTION('',(-1.,0.,0.));
#9753=DIRECTION('',(0.,0.,1.));
#9754=DIRECTION('',(1.,-1.23512438660689E-15,-2.69129956548782E-15));
#9755=DIRECTION('',(-2.69129956548782E-15,0.,-1.));
#9756=DIRECTION('',(1.,-1.18123916154475E-15,-1.96770129996799E-15));
#9757=DIRECTION('',(-1.96770129996799E-15,0.,-1.));
#9758=DIRECTION('',(1.,-1.24771907443915E-15,-1.41644362460478E-15));
#9759=DIRECTION('',(-1.41644362460478E-15,0.,-1.));
#9760=DIRECTION('',(1.,-1.4751360399877E-15,-1.19807507943364E-15));
#9761=DIRECTION('',(1.4751360399877E-15,1.,0.));
#9762=DIRECTION('',(1.,-2.04923588422118E-15,-1.13424025591296E-15));
#9763=DIRECTION('',(2.04923588422118E-15,1.,0.));
#9764=DIRECTION('',(1.,0.,0.));
#9765=DIRECTION('',(0.,0.,-1.));
#9766=DIRECTION('',(1.,-2.04923588422095E-15,-1.13424025591296E-15));
#9767=DIRECTION('',(2.04923588422095E-15,1.,0.));
#9768=DIRECTION('',(1.,-1.47513603998919E-15,-1.19807507943364E-15));
#9769=DIRECTION('',(1.47513603998919E-15,1.,0.));
#9770=DIRECTION('',(1.,-1.2477190744389E-15,-1.41644362460479E-15));
#9771=DIRECTION('',(-1.41644362460479E-15,0.,-1.));
#9772=DIRECTION('',(1.,-1.18123916154446E-15,-1.96770129996863E-15));
#9773=DIRECTION('',(-1.96770129996863E-15,0.,-1.));
#9774=DIRECTION('',(1.,-1.2477190744389E-15,-1.41644362460326E-15));
#9775=DIRECTION('',(-1.41644362460326E-15,0.,-1.));
#9776=DIRECTION('',(1.,-1.47513603998919E-15,-1.19807507943552E-15));
#9777=DIRECTION('',(1.47513603998919E-15,1.,0.));
#9778=DIRECTION('',(1.,-2.04923588422095E-15,-1.13424025591304E-15));
#9779=DIRECTION('',(2.04923588422095E-15,1.,0.));
#9780=DIRECTION('',(1.,0.,0.));
#9781=DIRECTION('',(0.,0.,-1.));
#9782=DIRECTION('',(1.,-2.04923588422118E-15,-1.13424025591304E-15));
#9783=DIRECTION('',(2.04923588422118E-15,1.,0.));
#9784=DIRECTION('',(1.,-1.4751360399877E-15,-1.19807507943551E-15));
#9785=DIRECTION('',(1.4751360399877E-15,1.,0.));
#9786=DIRECTION('',(1.,-1.24771907443915E-15,-1.41644362460326E-15));
#9787=DIRECTION('',(-1.41644362460326E-15,0.,-1.));
#9788=DIRECTION('',(1.,-1.18123916154475E-15,-1.96770129996863E-15));
#9789=DIRECTION('',(-1.96770129996863E-15,0.,-1.));
#9790=DIRECTION('',(-1.,-1.5350532643982E-16,1.45008721655328E-16));
#9791=DIRECTION('',(1.5350532643982E-16,-1.,0.));
#9792=DIRECTION('',(-1.,0.,0.));
#9793=DIRECTION('',(0.,0.,1.));
#9794=DIRECTION('',(-1.,0.,0.));
#9795=DIRECTION('',(0.,0.,1.));
#9796=DIRECTION('',(-0.866701294497581,-3.84892693049457E-16,-0.498827491339659));
#9797=DIRECTION('',(-4.44089209850063E-16,1.,0.));
#9798=DIRECTION('',(1.,0.,0.));
#9799=DIRECTION('',(0.,0.,-1.));
#9800=DIRECTION('',(1.,0.,0.));
#9801=DIRECTION('',(0.,0.,-1.));
#9802=DIRECTION('',(1.,0.,0.));
#9803=DIRECTION('',(0.,0.,-1.));
#9804=DIRECTION('',(-1.,-3.26422297091706E-17,-2.83054210170864E-17));
#9805=DIRECTION('',(3.26422297091706E-17,-1.,0.));
#9806=DIRECTION('',(1.,-1.52525712114884E-12,-4.12654899649895E-17));
#9807=DIRECTION('',(1.52525712114884E-12,1.,0.));
#9808=DIRECTION('',(1.,-2.17614864727806E-17,1.88702806780578E-17));
#9809=DIRECTION('',(2.17614864727806E-17,1.,0.));
#9810=DIRECTION('',(1.,1.01718677511461E-12,2.49678409077823E-17));
#9811=DIRECTION('',(-1.01718677511461E-12,1.,0.));
#9812=DIRECTION('',(1.,-1.52525712114884E-12,-4.12654899649895E-17));
#9813=DIRECTION('',(1.52525712114884E-12,1.,0.));
#9814=DIRECTION('',(1.,1.52523423639394E-12,4.77734628794545E-17));
#9815=DIRECTION('',(-1.52523423639394E-12,1.,0.));
#9816=DIRECTION('',(1.,1.01718677511461E-12,2.49678409077823E-17));
#9817=DIRECTION('',(-1.01718677511461E-12,1.,0.));
#9818=DIRECTION('',(1.,-1.01703038514308E-12,2.74738847694775E-17));
#9819=DIRECTION('',(1.01703038514308E-12,1.,0.));
#9820=DIRECTION('',(-1.,0.,-1.0449157878825E-16));
#9821=DIRECTION('',(-1.0449157878825E-16,0.,1.));
#9822=DIRECTION('',(-1.,0.,-1.0449157878825E-16));
#9823=DIRECTION('',(-1.0449157878825E-16,0.,1.));
#9824=DIRECTION('',(1.,1.5253472309144E-12,1.6070040430106E-17));
#9825=DIRECTION('',(-1.5253472309144E-12,1.,0.));
#9826=DIRECTION('',(1.,-1.52537011566931E-12,-9.71439789292615E-18));
#9827=DIRECTION('',(1.52537011566931E-12,1.,0.));
#9828=DIRECTION('',(-1.,8.77687473398116E-18,8.62198870926304E-18));
#9829=DIRECTION('',(-8.77687473398116E-18,-1.,0.));
#9830=DIRECTION('',(1.,-1.28458696201097E-12,-2.92084213202575E-17));
#9831=DIRECTION('',(1.28458696201097E-12,1.,0.));
#9832=DIRECTION('',(-1.,0.,-1.11022302462516E-16));
#9833=DIRECTION('',(-1.11022302462516E-16,0.,1.));
#9834=DIRECTION('',(-1.,0.,-1.11022302462516E-16));
#9835=DIRECTION('',(-1.11022302462516E-16,0.,1.));
#9836=DIRECTION('',(1.,-1.28458696201097E-12,-2.92084213202575E-17));
#9837=DIRECTION('',(1.28458696201097E-12,1.,0.));
#9838=DIRECTION('',(-1.,0.,0.));
#9839=DIRECTION('',(0.,0.,1.));
#9840=DIRECTION('',(1.,-1.06677650229913E-10,1.79070058553459E-17));
#9841=DIRECTION('',(1.06677650229913E-10,1.,0.));
#9842=DIRECTION('',(1.,1.06677627345158E-10,-7.52576163854158E-18));
#9843=DIRECTION('',(-1.06677627345158E-10,1.,0.));
#9844=DIRECTION('',(-1.,0.,-1.04189432305107E-15));
#9845=DIRECTION('',(-1.04189432305107E-15,0.,1.));
#9846=DIRECTION('',(-1.,0.,0.));
#9847=DIRECTION('',(0.,0.,1.));
#9848=DIRECTION('',(-1.,0.,0.));
#9849=DIRECTION('',(0.,0.,1.));
#9850=DIRECTION('',(-1.,0.,-1.04189432305107E-15));
#9851=DIRECTION('',(-1.04189432305107E-15,0.,1.));
#9852=DIRECTION('',(-1.,0.,-1.04189432305107E-15));
#9853=DIRECTION('',(-1.04189432305107E-15,0.,1.));
#9854=DIRECTION('',(1.,3.57212507207529E-11,7.69107850575555E-18));
#9855=DIRECTION('',(-3.57212507207529E-11,1.,0.));
#9856=DIRECTION('',(1.,3.57212507207529E-11,7.69107850575555E-18));
#9857=DIRECTION('',(-3.57212507207529E-11,1.,0.));
#9858=DIRECTION('',(1.,-3.57214956501127E-11,-1.55638472566498E-17));
#9859=DIRECTION('',(3.57214956501127E-11,1.,0.));
#9860=DIRECTION('',(1.,1.13344866900787E-10,1.0907594486052E-16));
#9861=DIRECTION('',(-1.13344866900787E-10,1.,0.));
#9862=DIRECTION('',(1.,-1.13344929948816E-10,-1.04122921954656E-16));
#9863=DIRECTION('',(1.13344929948816E-10,1.,0.));
#9864=DIRECTION('',(1.,-1.13344929948816E-10,-1.04122921954656E-16));
#9865=DIRECTION('',(1.13344929948816E-10,1.,0.));
#9866=DIRECTION('',(-1.,0.,2.61228946970625E-17));
#9867=DIRECTION('',(2.61228946970625E-17,0.,1.));
#9868=DIRECTION('',(-0.692635107763252,-3.07591777720995E-16,0.721288158431697));
#9869=DIRECTION('',(4.44089209850063E-16,-1.,0.));
#9870=DIRECTION('',(1.,0.,0.));
#9871=DIRECTION('',(0.,0.,-1.));
#9872=DIRECTION('',(1.,0.,0.));
#9873=DIRECTION('',(0.,0.,-1.));
#9874=DIRECTION('',(1.,0.,0.));
#9875=DIRECTION('',(0.,0.,-1.));
#9876=DIRECTION('',(-1.,-3.26422297091706E-17,-2.83054210170864E-17));
#9877=DIRECTION('',(3.26422297091706E-17,-1.,0.));
#9878=DIRECTION('',(1.,-1.52525712114884E-12,-4.12654899649895E-17));
#9879=DIRECTION('',(1.52525712114884E-12,1.,0.));
#9880=DIRECTION('',(1.,-2.37398034248512E-17,2.05857607396994E-17));
#9881=DIRECTION('',(2.37398034248512E-17,1.,0.));
#9882=DIRECTION('',(1.,1.1095485520975E-12,1.46545401316625E-17));
#9883=DIRECTION('',(-1.1095485520975E-12,1.,0.));
#9884=DIRECTION('',(1.,-1.52525712114884E-12,-4.12654899649895E-17));
#9885=DIRECTION('',(1.52525712114884E-12,1.,0.));
#9886=DIRECTION('',(1.,1.52523423639394E-12,4.77734628794545E-17));
#9887=DIRECTION('',(-1.52523423639394E-12,1.,0.));
#9888=DIRECTION('',(1.,1.1095485520975E-12,1.46545401316625E-17));
#9889=DIRECTION('',(-1.1095485520975E-12,1.,0.));
#9890=DIRECTION('',(1.,-1.10961798270237E-12,9.1670607747233E-18));
#9891=DIRECTION('',(1.10961798270237E-12,1.,0.));
#9892=DIRECTION('',(-1.,0.,-1.0449157878825E-16));
#9893=DIRECTION('',(-1.0449157878825E-16,0.,1.));
#9894=DIRECTION('',(-1.,0.,-1.0449157878825E-16));
#9895=DIRECTION('',(-1.0449157878825E-16,0.,1.));
#9896=DIRECTION('',(1.,1.5253472309144E-12,1.6070040430106E-17));
#9897=DIRECTION('',(-1.5253472309144E-12,1.,0.));
#9898=DIRECTION('',(1.,-1.52537011566931E-12,-9.71439789292615E-18));
#9899=DIRECTION('',(1.52537011566931E-12,1.,0.));
#9900=DIRECTION('',(-1.,9.57477243706982E-18,9.40580586465046E-18));
#9901=DIRECTION('',(-9.57477243706982E-18,-1.,0.));
#9902=DIRECTION('',(1.,-1.28458696201097E-12,-2.92084213202575E-17));
#9903=DIRECTION('',(1.28458696201097E-12,1.,0.));
#9904=DIRECTION('',(-1.,0.,-1.11022302462516E-16));
#9905=DIRECTION('',(-1.11022302462516E-16,0.,1.));
#9906=DIRECTION('',(-1.,0.,-1.11022302462516E-16));
#9907=DIRECTION('',(-1.11022302462516E-16,0.,1.));
#9908=DIRECTION('',(1.,-1.28458696201097E-12,-2.92084213202575E-17));
#9909=DIRECTION('',(1.28458696201097E-12,1.,0.));
#9910=DIRECTION('',(-1.,0.,0.));
#9911=DIRECTION('',(0.,0.,1.));
#9912=DIRECTION('',(1.,-1.06677650229913E-10,1.79070058553459E-17));
#9913=DIRECTION('',(1.06677650229913E-10,1.,0.));
#9914=DIRECTION('',(1.,1.06677627345158E-10,-7.52576163854158E-18));
#9915=DIRECTION('',(-1.06677627345158E-10,1.,0.));
#9916=DIRECTION('',(-1.,0.,-1.04189432305107E-15));
#9917=DIRECTION('',(-1.04189432305107E-15,0.,1.));
#9918=DIRECTION('',(-1.,0.,0.));
#9919=DIRECTION('',(0.,0.,1.));
#9920=DIRECTION('',(-1.,0.,0.));
#9921=DIRECTION('',(0.,0.,1.));
#9922=DIRECTION('',(-1.,0.,-1.04189432305107E-15));
#9923=DIRECTION('',(-1.04189432305107E-15,0.,1.));
#9924=DIRECTION('',(-1.,0.,-1.04189432305107E-15));
#9925=DIRECTION('',(-1.04189432305107E-15,0.,1.));
#9926=DIRECTION('',(1.,3.57212507207529E-11,7.69107850575555E-18));
#9927=DIRECTION('',(-3.57212507207529E-11,1.,0.));
#9928=DIRECTION('',(1.,3.57212507207529E-11,7.69107850575555E-18));
#9929=DIRECTION('',(-3.57212507207529E-11,1.,0.));
#9930=DIRECTION('',(1.,-3.57214956501127E-11,-1.55638472566498E-17));
#9931=DIRECTION('',(3.57214956501127E-11,1.,0.));
#9932=DIRECTION('',(1.,1.13344866900787E-10,1.0907594486052E-16));
#9933=DIRECTION('',(-1.13344866900787E-10,1.,0.));
#9934=DIRECTION('',(1.,-1.13344929948816E-10,-1.04122921954656E-16));
#9935=DIRECTION('',(1.13344929948816E-10,1.,0.));
#9936=DIRECTION('',(1.,-1.13344929948816E-10,-1.04122921954656E-16));
#9937=DIRECTION('',(1.13344929948816E-10,1.,0.));
#9938=DIRECTION('',(-1.,0.,2.61228946970625E-17));
#9939=DIRECTION('',(2.61228946970625E-17,0.,1.));
#9940=DIRECTION('',(0.537976075068644,2.38909370095472E-16,-0.842960107391647));
#9941=DIRECTION('',(-4.44089209850063E-16,1.,0.));
#9942=DIRECTION('',(1.,-4.75612924231451E-12,-4.0043073372981E-18));
#9943=DIRECTION('',(4.75612924231451E-12,1.,0.));
#9944=DIRECTION('',(1.,-4.75612924231451E-12,-4.0043073372981E-18));
#9945=DIRECTION('',(4.75612924231451E-12,1.,0.));
#9946=DIRECTION('',(1.,-4.75612924231451E-12,-4.0043073372981E-18));
#9947=DIRECTION('',(4.75612924231451E-12,1.,0.));
#9948=DIRECTION('',(1.,4.22825609356439E-17,-4.00585564781671E-17));
#9949=DIRECTION('',(-4.22825609356439E-17,1.,0.));
#9950=DIRECTION('',(1.,0.,-1.2509555207044E-16));
#9951=DIRECTION('',(-1.2509555207044E-16,0.,-1.));
#9952=DIRECTION('',(1.,0.,-7.40148683083438E-17));
#9953=DIRECTION('',(-7.40148683083438E-17,0.,-1.));
#9954=DIRECTION('',(1.,0.,-7.40148683083438E-17));
#9955=DIRECTION('',(-7.40148683083438E-17,0.,-1.));
#9956=DIRECTION('',(1.,0.,-1.2509555207044E-16));
#9957=DIRECTION('',(-1.2509555207044E-16,0.,-1.));
#9958=DIRECTION('',(1.,-8.51933299579803E-12,-1.51031137741696E-17));
#9959=DIRECTION('',(8.51933299579803E-12,1.,0.));
#9960=DIRECTION('',(1.,4.75611052379189E-12,2.67348976061206E-17));
#9961=DIRECTION('',(-4.75611052379189E-12,1.,0.));
#9962=DIRECTION('',(1.,4.75611052379189E-12,2.67348976061206E-17));
#9963=DIRECTION('',(-4.75611052379189E-12,1.,0.));
#9964=DIRECTION('',(1.,8.51931011104313E-12,9.10429714682885E-18));
#9965=DIRECTION('',(-8.51931011104313E-12,1.,0.));
#9966=DIRECTION('',(1.,-8.51933299579803E-12,-1.51031137741696E-17));
#9967=DIRECTION('',(8.51933299579803E-12,1.,0.));
#9968=DIRECTION('',(1.,-8.51933299579803E-12,-1.51031137741696E-17));
#9969=DIRECTION('',(8.51933299579803E-12,1.,0.));
#9970=DIRECTION('',(-1.,4.22825609356439E-17,4.00585564781671E-17));
#9971=DIRECTION('',(-4.22825609356439E-17,-1.,0.));
#9972=DIRECTION('',(1.,0.,0.));
#9973=DIRECTION('',(0.,0.,-1.));
#9974=DIRECTION('',(1.,0.,-7.90663281632159E-17));
#9975=DIRECTION('',(-7.90663281632159E-17,0.,-1.));
#9976=DIRECTION('',(1.,0.,-7.90663281632159E-17));
#9977=DIRECTION('',(-7.90663281632159E-17,0.,-1.));
#9978=DIRECTION('',(1.,0.,0.));
#9979=DIRECTION('',(0.,0.,-1.));
#9980=DIRECTION('',(1.,8.51953932343756E-12,7.17449131436051E-18));
#9981=DIRECTION('',(-8.51953932343756E-12,1.,0.));
#9982=DIRECTION('',(1.,5.87188086584048E-17,-5.56302802130048E-17));
#9983=DIRECTION('',(-5.87188086584048E-17,1.,0.));
#9984=DIRECTION('',(1.,-7.13444545520919E-12,-2.65134118218329E-17));
#9985=DIRECTION('',(7.13444545520919E-12,1.,0.));
#9986=DIRECTION('',(1.,7.13442257045429E-12,2.86761022065096E-17));
#9987=DIRECTION('',(-7.13442257045429E-12,1.,0.));
#9988=DIRECTION('',(1.,-8.51956220819246E-12,-1.01389396052301E-18));
#9989=DIRECTION('',(8.51956220819246E-12,1.,0.));
#9990=DIRECTION('',(1.,8.51953932343756E-12,7.17449131436051E-18));
#9991=DIRECTION('',(-8.51953932343756E-12,1.,0.));
#9992=DIRECTION('',(1.,8.51953932343756E-12,7.17449131436051E-18));
#9993=DIRECTION('',(-8.51953932343756E-12,1.,0.));
#9994=DIRECTION('',(1.,7.13442257045429E-12,2.86761022065096E-17));
#9995=DIRECTION('',(-7.13442257045429E-12,1.,0.));
#9996=DIRECTION('',(1.,-7.13444545520919E-12,-2.65134118218329E-17));
#9997=DIRECTION('',(7.13444545520919E-12,1.,0.));
#9998=DIRECTION('',(1.,-7.13444545520919E-12,-2.65134118218329E-17));
#9999=DIRECTION('',(7.13444545520919E-12,1.,0.));
#10000=DIRECTION('',(1.,0.,0.));
#10001=DIRECTION('',(0.,0.,-1.));
#10002=DIRECTION('',(1.,0.,0.));
#10003=DIRECTION('',(0.,0.,-1.));
#10004=DIRECTION('',(1.,0.,-1.1842378929335E-16));
#10005=DIRECTION('',(-1.1842378929335E-16,0.,-1.));
#10006=DIRECTION('',(1.,7.13444719404544E-12,-2.88724849698279E-17));
#10007=DIRECTION('',(-7.13444719404544E-12,1.,0.));
#10008=DIRECTION('',(-1.,5.58989788640793E-17,5.29587695813052E-17));
#10009=DIRECTION('',(-5.58989788640793E-17,-1.,0.));
#10010=DIRECTION('',(1.,7.13444719404544E-12,-2.88724849698279E-17));
#10011=DIRECTION('',(-7.13444719404544E-12,1.,0.));
#10012=DIRECTION('',(1.,-7.13447007880035E-12,4.01455929805839E-17));
#10013=DIRECTION('',(7.13447007880035E-12,1.,0.));
#10014=DIRECTION('',(1.,-7.13447007880035E-12,4.01455929805839E-17));
#10015=DIRECTION('',(7.13447007880035E-12,1.,0.));
#10016=DIRECTION('',(1.,7.13444719404544E-12,-2.88724849698279E-17));
#10017=DIRECTION('',(-7.13444719404544E-12,1.,0.));
#10018=DIRECTION('',(-0.871054783314631,-3.86826030458312E-16,0.491185875677122));
#10019=DIRECTION('',(4.44089209850063E-16,-1.,0.));
#10020=DIRECTION('',(1.,-4.75612924231451E-12,-4.0043073372981E-18));
#10021=DIRECTION('',(4.75612924231451E-12,1.,0.));
#10022=DIRECTION('',(1.,-4.75612924231451E-12,-4.0043073372981E-18));
#10023=DIRECTION('',(4.75612924231451E-12,1.,0.));
#10024=DIRECTION('',(1.,-4.75612924231451E-12,-4.0043073372981E-18));
#10025=DIRECTION('',(4.75612924231451E-12,1.,0.));
#10026=DIRECTION('',(1.,4.22825609356439E-17,-4.00585564781671E-17));
#10027=DIRECTION('',(-4.22825609356439E-17,1.,0.));
#10028=DIRECTION('',(1.,0.,-1.2509555207044E-16));
#10029=DIRECTION('',(-1.2509555207044E-16,0.,-1.));
#10030=DIRECTION('',(1.,0.,-7.40148683083438E-17));
#10031=DIRECTION('',(-7.40148683083438E-17,0.,-1.));
#10032=DIRECTION('',(1.,0.,-7.40148683083438E-17));
#10033=DIRECTION('',(-7.40148683083438E-17,0.,-1.));
#10034=DIRECTION('',(1.,0.,-1.2509555207044E-16));
#10035=DIRECTION('',(-1.2509555207044E-16,0.,-1.));
#10036=DIRECTION('',(1.,-8.51933299579803E-12,-1.51031137741696E-17));
#10037=DIRECTION('',(8.51933299579803E-12,1.,0.));
#10038=DIRECTION('',(1.,4.75611052379189E-12,2.67348976061206E-17));
#10039=DIRECTION('',(-4.75611052379189E-12,1.,0.));
#10040=DIRECTION('',(1.,4.75611052379189E-12,2.67348976061206E-17));
#10041=DIRECTION('',(-4.75611052379189E-12,1.,0.));
#10042=DIRECTION('',(1.,8.51931011104313E-12,9.10429714682885E-18));
#10043=DIRECTION('',(-8.51931011104313E-12,1.,0.));
#10044=DIRECTION('',(1.,-8.51933299579803E-12,-1.51031137741696E-17));
#10045=DIRECTION('',(8.51933299579803E-12,1.,0.));
#10046=DIRECTION('',(1.,-8.51933299579803E-12,-1.51031137741696E-17));
#10047=DIRECTION('',(8.51933299579803E-12,1.,0.));
#10048=DIRECTION('',(-1.,4.22825609356439E-17,4.00585564781671E-17));
#10049=DIRECTION('',(-4.22825609356439E-17,-1.,0.));
#10050=DIRECTION('',(1.,0.,0.));
#10051=DIRECTION('',(0.,0.,-1.));
#10052=DIRECTION('',(1.,0.,-7.90663281632159E-17));
#10053=DIRECTION('',(-7.90663281632159E-17,0.,-1.));
#10054=DIRECTION('',(1.,0.,-7.90663281632159E-17));
#10055=DIRECTION('',(-7.90663281632159E-17,0.,-1.));
#10056=DIRECTION('',(1.,0.,0.));
#10057=DIRECTION('',(0.,0.,-1.));
#10058=DIRECTION('',(1.,8.51953932343756E-12,7.17449131436051E-18));
#10059=DIRECTION('',(-8.51953932343756E-12,1.,0.));
#10060=DIRECTION('',(1.,5.87188086584048E-17,-5.56302802130048E-17));
#10061=DIRECTION('',(-5.87188086584048E-17,1.,0.));
#10062=DIRECTION('',(1.,-7.13444545520919E-12,-2.65134118218329E-17));
#10063=DIRECTION('',(7.13444545520919E-12,1.,0.));
#10064=DIRECTION('',(1.,7.13442257045429E-12,2.86761022065096E-17));
#10065=DIRECTION('',(-7.13442257045429E-12,1.,0.));
#10066=DIRECTION('',(1.,-8.51956220819246E-12,-1.01389396052301E-18));
#10067=DIRECTION('',(8.51956220819246E-12,1.,0.));
#10068=DIRECTION('',(1.,8.51953932343756E-12,7.17449131436051E-18));
#10069=DIRECTION('',(-8.51953932343756E-12,1.,0.));
#10070=DIRECTION('',(1.,8.51953932343756E-12,7.17449131436051E-18));
#10071=DIRECTION('',(-8.51953932343756E-12,1.,0.));
#10072=DIRECTION('',(1.,7.13442257045429E-12,2.86761022065096E-17));
#10073=DIRECTION('',(-7.13442257045429E-12,1.,0.));
#10074=DIRECTION('',(1.,-7.13444545520919E-12,-2.65134118218329E-17));
#10075=DIRECTION('',(7.13444545520919E-12,1.,0.));
#10076=DIRECTION('',(1.,-7.13444545520919E-12,-2.65134118218329E-17));
#10077=DIRECTION('',(7.13444545520919E-12,1.,0.));
#10078=DIRECTION('',(1.,0.,0.));
#10079=DIRECTION('',(0.,0.,-1.));
#10080=DIRECTION('',(1.,0.,0.));
#10081=DIRECTION('',(0.,0.,-1.));
#10082=DIRECTION('',(1.,0.,-1.1842378929335E-16));
#10083=DIRECTION('',(-1.1842378929335E-16,0.,-1.));
#10084=DIRECTION('',(1.,7.13444719404544E-12,-2.88724849698279E-17));
#10085=DIRECTION('',(-7.13444719404544E-12,1.,0.));
#10086=DIRECTION('',(-1.,5.58989788640793E-17,5.29587695813052E-17));
#10087=DIRECTION('',(-5.58989788640793E-17,-1.,0.));
#10088=DIRECTION('',(1.,7.13444719404544E-12,-2.88724849698279E-17));
#10089=DIRECTION('',(-7.13444719404544E-12,1.,0.));
#10090=DIRECTION('',(1.,-7.13447007880035E-12,4.01455929805839E-17));
#10091=DIRECTION('',(7.13447007880035E-12,1.,0.));
#10092=DIRECTION('',(1.,-7.13447007880035E-12,4.01455929805839E-17));
#10093=DIRECTION('',(7.13447007880035E-12,1.,0.));
#10094=DIRECTION('',(1.,7.13444719404544E-12,-2.88724849698279E-17));
#10095=DIRECTION('',(-7.13444719404544E-12,1.,0.));
#10096=DIRECTION('',(-0.121354390358123,-5.38921753259749E-17,-0.99260924433576));
#10097=DIRECTION('',(-4.44089209850063E-16,1.,0.));
#10098=DIRECTION('',(1.,0.,0.));
#10099=DIRECTION('',(0.,0.,-1.));
#10100=DIRECTION('',(1.,0.,0.));
#10101=DIRECTION('',(0.,0.,-1.));
#10102=DIRECTION('',(1.,0.,0.));
#10103=DIRECTION('',(0.,0.,-1.));
#10104=DIRECTION('',(1.,2.02801224290451E-16,-2.41603252256269E-16));
#10105=DIRECTION('',(-2.41603252256269E-16,0.,-1.));
#10106=DIRECTION('',(-1.,0.,0.));
#10107=DIRECTION('',(0.,0.,1.));
#10108=DIRECTION('',(-1.,0.,2.12198590438362E-17));
#10109=DIRECTION('',(2.12198590438362E-17,0.,1.));
#10110=DIRECTION('',(-1.,0.,0.));
#10111=DIRECTION('',(0.,0.,1.));
#10112=DIRECTION('',(-1.,0.,0.));
#10113=DIRECTION('',(0.,0.,1.));
#10114=DIRECTION('',(-1.,0.,0.));
#10115=DIRECTION('',(0.,0.,1.));
#10116=DIRECTION('',(-1.,0.,0.));
#10117=DIRECTION('',(0.,0.,1.));
#10118=DIRECTION('',(-1.,0.,0.));
#10119=DIRECTION('',(0.,0.,1.));
#10120=DIRECTION('',(-1.,-4.24397180875387E-17,-5.66873377313974E-17));
#10121=DIRECTION('',(-5.66873377313974E-17,0.,1.));
#10122=DIRECTION('',(1.,0.,0.));
#10123=DIRECTION('',(0.,0.,-1.));
#10124=DIRECTION('',(1.,1.03977309314787E-16,-1.08221281123575E-16));
#10125=DIRECTION('',(-1.08221281123575E-16,0.,-1.));
#10126=DIRECTION('',(1.,0.,0.));
#10127=DIRECTION('',(0.,0.,-1.));
#10128=DIRECTION('',(1.,0.,0.));
#10129=DIRECTION('',(0.,0.,-1.));
#10130=DIRECTION('',(1.,0.,0.));
#10131=DIRECTION('',(0.,0.,-1.));
#10132=DIRECTION('',(1.,0.,0.));
#10133=DIRECTION('',(0.,0.,-1.));
#10134=DIRECTION('',(1.,0.,0.));
#10135=DIRECTION('',(0.,0.,-1.));
#10136=DIRECTION('',(1.,5.72936194184529E-17,-1.22772041610769E-16));
#10137=DIRECTION('',(-1.22772041610769E-16,0.,-1.));
#10138=DIRECTION('',(-1.,0.,0.));
#10139=DIRECTION('',(0.,0.,1.));
#10140=DIRECTION('',(-1.,6.82066897833321E-18,2.57669716961208E-18));
#10141=DIRECTION('',(-6.82066897833321E-18,-1.,0.));
#10142=DIRECTION('',(-1.,0.,0.));
#10143=DIRECTION('',(0.,0.,1.));
#10144=DIRECTION('',(-1.,0.,0.));
#10145=DIRECTION('',(0.,0.,1.));
#10146=DIRECTION('',(-1.,0.,0.));
#10147=DIRECTION('',(0.,0.,1.));
#10148=DIRECTION('',(-1.,0.,0.));
#10149=DIRECTION('',(0.,0.,1.));
#10150=DIRECTION('',(-1.,0.,0.));
#10151=DIRECTION('',(0.,0.,1.));
#10152=DIRECTION('',(-1.,7.12380982182306E-18,-2.27355632612368E-18));
#10153=DIRECTION('',(-7.12380982182306E-18,-1.,0.));
#10154=DIRECTION('',(1.,0.,0.));
#10155=DIRECTION('',(0.,0.,-1.));
#10156=DIRECTION('',(1.,2.91015209743734E-17,4.57742673659912E-17));
#10157=DIRECTION('',(4.57742673659912E-17,0.,-1.));
#10158=DIRECTION('',(1.,0.,0.));
#10159=DIRECTION('',(0.,0.,-1.));
#10160=DIRECTION('',(1.,0.,0.));
#10161=DIRECTION('',(0.,0.,-1.));
#10162=DIRECTION('',(1.,0.,0.));
#10163=DIRECTION('',(0.,0.,-1.));
#10164=DIRECTION('',(1.,0.,0.));
#10165=DIRECTION('',(0.,0.,-1.));
#10166=DIRECTION('',(1.,0.,0.));
#10167=DIRECTION('',(0.,0.,-1.));
#10168=DIRECTION('',(1.,7.27538024359589E-17,-9.63987882277241E-17));
#10169=DIRECTION('',(-9.63987882277241E-17,0.,-1.));
#10170=DIRECTION('',(-1.,0.,0.));
#10171=DIRECTION('',(0.,0.,1.));
#10172=DIRECTION('',(-1.,-6.66909855658537E-18,-5.75967602618571E-18));
#10173=DIRECTION('',(6.66909855658537E-18,-1.,0.));
#10174=DIRECTION('',(-1.,0.,0.));
#10175=DIRECTION('',(0.,0.,1.));
#10176=DIRECTION('',(-1.,0.,0.));
#10177=DIRECTION('',(0.,0.,1.));
#10178=DIRECTION('',(-1.,0.,0.));
#10179=DIRECTION('',(0.,0.,1.));
#10180=DIRECTION('',(-1.,0.,0.));
#10181=DIRECTION('',(0.,0.,1.));
#10182=DIRECTION('',(-1.,0.,0.));
#10183=DIRECTION('',(0.,0.,1.));
#10184=DIRECTION('',(-1.,2.5009119587355E-17,1.22772041610769E-17));
#10185=DIRECTION('',(-2.5009119587355E-17,-1.,0.));
#10186=DIRECTION('',(1.,0.,0.));
#10187=DIRECTION('',(0.,0.,-1.));
#10188=DIRECTION('',(1.,2.4205796352152E-16,-2.29326048095192E-16));
#10189=DIRECTION('',(-2.4205796352152E-16,1.,0.));
#10190=DIRECTION('',(1.,0.,0.));
#10191=DIRECTION('',(0.,0.,-1.));
#10192=DIRECTION('',(1.,0.,0.));
#10193=DIRECTION('',(0.,0.,-1.));
#10194=DIRECTION('',(1.,0.,0.));
#10195=DIRECTION('',(0.,0.,-1.));
#10196=DIRECTION('',(1.,0.,0.));
#10197=DIRECTION('',(0.,0.,-1.));
#10198=DIRECTION('',(1.,0.,0.));
#10199=DIRECTION('',(0.,0.,-1.));
#10200=DIRECTION('',(1.,1.58886509469999E-16,-1.7842870047433E-16));
#10201=DIRECTION('',(-1.7842870047433E-16,0.,-1.));
#10202=DIRECTION('',(-1.,0.,0.));
#10203=DIRECTION('',(0.,0.,1.));
#10204=DIRECTION('',(1.,0.,0.));
#10205=DIRECTION('',(0.,0.,-1.));
#10206=DIRECTION('',(1.,0.,0.));
#10207=DIRECTION('',(0.,0.,-1.));
#10208=DIRECTION('',(-1.,0.,0.));
#10209=DIRECTION('',(0.,0.,1.));
#10210=DIRECTION('',(-1.,0.,0.));
#10211=DIRECTION('',(0.,0.,1.));
#10212=DIRECTION('',(1.,0.,0.));
#10213=DIRECTION('',(0.,0.,-1.));
#10214=DIRECTION('',(1.,0.,0.));
#10215=DIRECTION('',(0.,0.,-1.));
#10216=DIRECTION('',(-1.,-5.92083225297793E-17,-6.5638185609928E-17));
#10217=DIRECTION('',(-6.5638185609928E-17,0.,1.));
#10218=DIRECTION('',(-1.,0.,0.));
#10219=DIRECTION('',(0.,0.,1.));
#10220=DIRECTION('',(1.,2.03904353819831E-16,-2.22341986202179E-16));
#10221=DIRECTION('',(-2.22341986202179E-16,0.,-1.));
#10222=DIRECTION('',(1.,0.,0.));
#10223=DIRECTION('',(0.,0.,-1.));
#10224=DIRECTION('',(-1.,0.,0.));
#10225=DIRECTION('',(0.,0.,1.));
#10226=DIRECTION('',(-1.,0.,0.));
#10227=DIRECTION('',(0.,0.,1.));
#10228=DIRECTION('',(1.,0.,0.));
#10229=DIRECTION('',(0.,0.,-1.));
#10230=DIRECTION('',(-1.,0.,0.));
#10231=DIRECTION('',(0.,0.,1.));
#10232=DIRECTION('',(-1.,-8.42579974462088E-17,-9.46212805545689E-17));
#10233=DIRECTION('',(-9.46212805545689E-17,0.,1.));
#10234=DIRECTION('',(1.,-1.27665164684106E-12,-1.01285822605064E-16));
#10235=DIRECTION('',(1.27665164684106E-12,1.,0.));
#10236=DIRECTION('',(1.,0.,0.));
#10237=DIRECTION('',(0.,0.,-1.));
#10238=DIRECTION('',(1.,0.,0.));
#10239=DIRECTION('',(0.,0.,-1.));
#10240=DIRECTION('',(1.,0.,0.));
#10241=DIRECTION('',(0.,0.,-1.));
#10242=DIRECTION('',(1.,0.,0.));
#10243=DIRECTION('',(0.,0.,-1.));
#10244=DIRECTION('',(1.,0.,0.));
#10245=DIRECTION('',(0.,0.,-1.));
#10246=DIRECTION('',(1.,0.,0.));
#10247=DIRECTION('',(0.,0.,-1.));
#10248=DIRECTION('',(1.,0.,0.));
#10249=DIRECTION('',(0.,0.,-1.));
#10250=DIRECTION('',(1.,0.,0.));
#10251=DIRECTION('',(0.,0.,-1.));
#10252=DIRECTION('',(1.,0.,0.));
#10253=DIRECTION('',(0.,0.,-1.));
#10254=DIRECTION('',(1.,0.,0.));
#10255=DIRECTION('',(0.,0.,-1.));
#10256=DIRECTION('',(1.,0.,0.));
#10257=DIRECTION('',(0.,0.,-1.));
#10258=DIRECTION('',(1.,0.,0.));
#10259=DIRECTION('',(0.,0.,-1.));
#10260=DIRECTION('',(1.,0.,0.));
#10261=DIRECTION('',(0.,0.,-1.));
#10262=DIRECTION('',(1.,0.,0.));
#10263=DIRECTION('',(0.,0.,-1.));
#10264=DIRECTION('',(1.,0.,0.));
#10265=DIRECTION('',(0.,0.,-1.));
#10266=DIRECTION('',(1.,0.,0.));
#10267=DIRECTION('',(0.,0.,-1.));
#10268=DIRECTION('',(1.,0.,0.));
#10269=DIRECTION('',(0.,0.,-1.));
#10270=DIRECTION('',(1.,0.,0.));
#10271=DIRECTION('',(0.,0.,-1.));
#10272=DIRECTION('',(-1.,0.,0.));
#10273=DIRECTION('',(0.,0.,1.));
#10274=DIRECTION('',(1.,0.,0.));
#10275=DIRECTION('',(0.,0.,-1.));
#10276=DIRECTION('',(1.,0.,0.));
#10277=DIRECTION('',(0.,0.,-1.));
#10278=DIRECTION('',(1.,0.,0.));
#10279=DIRECTION('',(0.,0.,-1.));
#10280=DIRECTION('',(1.,0.,0.));
#10281=DIRECTION('',(0.,0.,-1.));
#10282=DIRECTION('',(1.,0.,0.));
#10283=DIRECTION('',(0.,0.,-1.));
#10284=DIRECTION('',(1.,0.,0.));
#10285=DIRECTION('',(0.,0.,-1.));
#10286=DIRECTION('',(1.,0.,0.));
#10287=DIRECTION('',(0.,0.,-1.));
#10288=DIRECTION('',(1.,0.,0.));
#10289=DIRECTION('',(0.,0.,-1.));
#10290=DIRECTION('',(1.,0.,0.));
#10291=DIRECTION('',(0.,0.,-1.));
#10292=DIRECTION('',(1.,0.,0.));
#10293=DIRECTION('',(0.,0.,-1.));
#10294=DIRECTION('',(1.,0.,0.));
#10295=DIRECTION('',(0.,0.,-1.));
#10296=DIRECTION('',(1.,0.,0.));
#10297=DIRECTION('',(0.,0.,-1.));
#10298=DIRECTION('',(1.,0.,0.));
#10299=DIRECTION('',(0.,0.,-1.));
#10300=DIRECTION('',(1.,0.,0.));
#10301=DIRECTION('',(0.,0.,-1.));
#10302=DIRECTION('',(1.,0.,0.));
#10303=DIRECTION('',(0.,0.,-1.));
#10304=DIRECTION('',(1.,0.,0.));
#10305=DIRECTION('',(0.,0.,-1.));
#10306=DIRECTION('',(1.,0.,0.));
#10307=DIRECTION('',(0.,0.,-1.));
#10308=DIRECTION('',(1.,0.,0.));
#10309=DIRECTION('',(0.,0.,-1.));
#10310=DIRECTION('',(1.,0.,0.));
#10311=DIRECTION('',(0.,0.,-1.));
#10312=DIRECTION('',(1.,0.,0.));
#10313=DIRECTION('',(0.,0.,-1.));
#10314=DIRECTION('',(1.,0.,0.));
#10315=DIRECTION('',(0.,0.,-1.));
#10316=DIRECTION('',(1.,0.,0.));
#10317=DIRECTION('',(0.,0.,-1.));
#10318=DIRECTION('',(1.,0.,0.));
#10319=DIRECTION('',(0.,0.,-1.));
#10320=DIRECTION('',(1.,0.,0.));
#10321=DIRECTION('',(0.,0.,-1.));
#10322=DIRECTION('',(1.,0.,0.));
#10323=DIRECTION('',(0.,0.,-1.));
#10324=DIRECTION('',(1.,0.,0.));
#10325=DIRECTION('',(0.,0.,-1.));
#10326=DIRECTION('',(1.,0.,0.));
#10327=DIRECTION('',(0.,0.,-1.));
#10328=DIRECTION('',(1.,0.,0.));
#10329=DIRECTION('',(0.,0.,-1.));
#10330=DIRECTION('',(1.,0.,0.));
#10331=DIRECTION('',(0.,0.,-1.));
#10332=DIRECTION('',(1.,0.,0.));
#10333=DIRECTION('',(0.,0.,-1.));
#10334=DIRECTION('',(1.,0.,0.));
#10335=DIRECTION('',(0.,0.,-1.));
#10336=DIRECTION('',(1.,0.,0.));
#10337=DIRECTION('',(0.,0.,-1.));
#10338=DIRECTION('',(1.,0.,0.));
#10339=DIRECTION('',(0.,0.,-1.));
#10340=DIRECTION('',(1.,0.,0.));
#10341=DIRECTION('',(0.,0.,-1.));
#10342=DIRECTION('',(1.,0.,0.));
#10343=DIRECTION('',(0.,0.,-1.));
#10344=DIRECTION('',(1.,0.,0.));
#10345=DIRECTION('',(0.,0.,-1.));
#10346=DIRECTION('',(1.,0.,0.));
#10347=DIRECTION('',(0.,0.,-1.));
#10348=DIRECTION('',(1.,-1.27665164684106E-12,-1.01285822605064E-16));
#10349=DIRECTION('',(1.27665164684106E-12,1.,0.));
#10350=DIRECTION('',(1.,1.27662876208615E-12,9.94459735806396E-17));
#10351=DIRECTION('',(-1.27662876208615E-12,1.,0.));
#10352=DIRECTION('',(1.,0.,0.));
#10353=DIRECTION('',(0.,0.,-1.));
#10354=DIRECTION('',(1.,0.,0.));
#10355=DIRECTION('',(0.,0.,-1.));
#10356=DIRECTION('',(1.,1.00478788398415E-16,-1.1970342952697E-16));
#10357=DIRECTION('',(-1.1970342952697E-16,0.,-1.));
#10358=DIRECTION('',(1.,1.27681490610412E-12,3.06367665504718E-17));
#10359=DIRECTION('',(-1.27681490610412E-12,1.,0.));
#10360=DIRECTION('',(-1.,0.,0.));
#10361=DIRECTION('',(0.,0.,1.));
#10362=DIRECTION('',(-1.,0.,0.));
#10363=DIRECTION('',(0.,0.,1.));
#10364=DIRECTION('',(-1.,0.,0.));
#10365=DIRECTION('',(0.,0.,1.));
#10366=DIRECTION('',(1.,0.,0.));
#10367=DIRECTION('',(0.,0.,-1.));
#10368=DIRECTION('',(1.,0.,0.));
#10369=DIRECTION('',(0.,0.,-1.));
#10370=DIRECTION('',(-1.,0.,0.));
#10371=DIRECTION('',(0.,0.,1.));
#10372=DIRECTION('',(1.,1.27681490610412E-12,3.06367665504718E-17));
#10373=DIRECTION('',(-1.27681490610412E-12,1.,0.));
#10374=DIRECTION('',(1.,0.,0.));
#10375=DIRECTION('',(0.,0.,-1.));
#10376=DIRECTION('',(1.,0.,0.));
#10377=DIRECTION('',(0.,0.,-1.));
#10378=DIRECTION('',(1.,0.,0.));
#10379=DIRECTION('',(0.,0.,-1.));
#10380=DIRECTION('',(1.,0.,0.));
#10381=DIRECTION('',(0.,0.,-1.));
#10382=DIRECTION('',(-1.,3.16611816286098E-16,2.99958470908511E-16));
#10383=DIRECTION('',(-3.16611816286098E-16,-1.,0.));
#10384=DIRECTION('',(1.,0.,0.));
#10385=DIRECTION('',(0.,0.,-1.));
#10386=DIRECTION('',(1.,-6.10766397547714E-11,6.58357325455797E-17));
#10387=DIRECTION('',(6.10766397547714E-11,1.,0.));
#10388=DIRECTION('',(-1.,0.,-2.21547530017009E-16));
#10389=DIRECTION('',(-2.21547530017009E-16,0.,1.));
#10390=DIRECTION('',(1.,6.10765954034213E-11,-7.15867759341588E-17));
#10391=DIRECTION('',(-6.10765954034213E-11,1.,0.));
#10392=DIRECTION('',(1.,0.,0.));
#10393=DIRECTION('',(0.,0.,-1.));
#10394=DIRECTION('',(1.,4.34750133448528E-12,-7.07356447213086E-17));
#10395=DIRECTION('',(-4.34750133448528E-12,1.,0.));
#10396=DIRECTION('',(-1.,0.,-2.21547530017009E-16));
#10397=DIRECTION('',(-2.21547530017009E-16,0.,1.));
#10398=DIRECTION('',(-1.,0.,-2.21547530017009E-16));
#10399=DIRECTION('',(-2.21547530017009E-16,0.,1.));
#10400=DIRECTION('',(-1.,0.,-2.21547530017009E-16));
#10401=DIRECTION('',(-2.21547530017009E-16,0.,1.));
#10402=DIRECTION('',(1.,4.34750133448528E-12,-7.07356447213086E-17));
#10403=DIRECTION('',(-4.34750133448528E-12,1.,0.));
#10404=DIRECTION('',(1.,4.34750133448528E-12,-7.07356447213086E-17));
#10405=DIRECTION('',(-4.34750133448528E-12,1.,0.));
#10406=DIRECTION('',(1.,1.75950681255562E-16,1.77784902179881E-11));
#10407=DIRECTION('',(1.77784902179881E-11,0.,-1.));
#10408=DIRECTION('',(-1.,0.,0.));
#10409=DIRECTION('',(0.,0.,1.));
#10410=DIRECTION('',(0.094639757655587,0.973920700489943,0.206208111935661));
#10411=DIRECTION('',(0.,-0.2071378324481,0.978311769513534));
#10412=DIRECTION('',(1.,8.1117015446827E-11,-1.3991198231814E-10));
#10413=DIRECTION('',(-1.3991198231814E-10,0.,-1.));
#10414=DIRECTION('',(1.,8.1117015446827E-11,-1.3991198231814E-10));
#10415=DIRECTION('',(-1.3991198231814E-10,0.,-1.));
#10416=DIRECTION('',(-0.0946398168959535,0.665538133586411,0.740339312612951));
#10417=DIRECTION('',(0.,-0.743677248769676,0.668538816870319));
#10418=DIRECTION('',(1.,-4.95011636935677E-10,2.85369859870056E-10));
#10419=DIRECTION('',(4.95011636935677E-10,1.,0.));
#10420=DIRECTION('',(0.0946397575924438,0.308378887082395,0.946544123791737));
#10421=DIRECTION('',(0.,-0.9508117613661,0.309769260011214));
#10422=DIRECTION('',(1.,1.17652320289254E-10,4.87112968899379E-16));
#10423=DIRECTION('',(-1.17652320289254E-10,1.,0.));
#10424=DIRECTION('',(1.,1.17652320289254E-10,4.87112968899379E-16));
#10425=DIRECTION('',(-1.17652320289254E-10,1.,0.));
#10426=DIRECTION('',(-0.0946398171021046,-0.308383585244705,0.946542587193256));
#10427=DIRECTION('',(0.,-0.950810223242973,-0.30977398111631));
#10428=DIRECTION('',(1.,-4.95007884417356E-10,-2.85368119247311E-10));
#10429=DIRECTION('',(4.95007884417356E-10,1.,0.));
#10430=DIRECTION('',(0.0946397579762018,-0.66554181379473,0.740336011754816));
#10431=DIRECTION('',(0.,-0.743673928844786,-0.668542509909848));
#10432=DIRECTION('',(1.,8.11172698461387E-11,1.39913973791465E-10));
#10433=DIRECTION('',(1.39913973791465E-10,0.,-1.));
#10434=DIRECTION('',(1.,8.11172698461387E-11,1.39913973791465E-10));
#10435=DIRECTION('',(1.39913973791465E-10,0.,-1.));
#10436=DIRECTION('',(0.094639816908078,0.973921718912833,-0.206203274672052));
#10437=DIRECTION('',(0.,0.20713297454698,0.978312798063748));
#10438=DIRECTION('',(1.,-4.74005497252645E-11,-6.27882181535306E-10));
#10439=DIRECTION('',(-6.27882181535306E-10,0.,-1.));
#10440=DIRECTION('',(-4.739727861225E-11,1.,-8.7405760717612E-11));
#10441=DIRECTION('',(0.,8.7405760717612E-11,1.));
#10442=DIRECTION('',(1.,4.73972785573744E-11,-6.27826053903067E-10));
#10443=DIRECTION('',(-6.27826053903067E-10,0.,-1.));
#10444=DIRECTION('',(-0.0946397577561541,0.973920700463518,0.206208112014312));
#10445=DIRECTION('',(0.,-0.207137832529095,0.978311769496385));
#10446=DIRECTION('',(1.,-8.11134369730464E-11,1.39906722256238E-10));
#10447=DIRECTION('',(1.39906722256238E-10,0.,-1.));
#10448=DIRECTION('',(1.,-8.11134369730464E-11,1.39906722256238E-10));
#10449=DIRECTION('',(1.39906722256238E-10,0.,-1.));
#10450=DIRECTION('',(0.094639817014141,0.665538133630341,0.740339312558352));
#10451=DIRECTION('',(0.,-0.743677248723224,0.668538816921992));
#10452=DIRECTION('',(1.,4.95010500146808E-10,-2.8536921183499E-10));
#10453=DIRECTION('',(-4.95010500146808E-10,1.,0.));
#10454=DIRECTION('',(-0.094639757574348,0.308378887070613,0.946544123797385));
#10455=DIRECTION('',(0.,-0.95081176137013,0.309769259998844));
#10456=DIRECTION('',(1.,-1.17647616855165E-10,2.02965890778723E-16));
#10457=DIRECTION('',(1.17647616855165E-10,1.,0.));
#10458=DIRECTION('',(1.,-1.17647616855165E-10,2.02965890778723E-16));
#10459=DIRECTION('',(1.17647616855165E-10,1.,0.));
#10460=DIRECTION('',(0.0946398171021004,-0.308383585244707,0.946542587193255));
#10461=DIRECTION('',(0.,-0.950810223242972,-0.309773981116312));
#10462=DIRECTION('',(1.,4.95008651459005E-10,2.85368745562457E-10));
#10463=DIRECTION('',(-4.95008651459005E-10,1.,0.));
#10464=DIRECTION('',(-0.094639757976208,-0.665541813794729,0.740336011754816));
#10465=DIRECTION('',(0.,-0.743673928844787,-0.668542509909848));
#10466=DIRECTION('',(1.,-8.11137982698219E-11,-1.3990738019364E-10));
#10467=DIRECTION('',(-1.3990738019364E-10,0.,-1.));
#10468=DIRECTION('',(1.,-8.11137982698219E-11,-1.3990738019364E-10));
#10469=DIRECTION('',(-1.3990738019364E-10,0.,-1.));
#10470=DIRECTION('',(-0.0946398169083375,0.973921718912779,-0.206203274672188));
#10471=DIRECTION('',(0.,0.207132974547121,0.978312798063718));
#10472=DIRECTION('',(1.,-6.96086070235072E-17,7.71679127636215E-17));
#10473=DIRECTION('',(7.71679127636215E-17,0.,-1.));
#10474=DIRECTION('',(1.,3.14873594454048E-12,1.4723392451601E-16));
#10475=DIRECTION('',(-3.14873594454048E-12,1.,0.));
#10476=DIRECTION('',(-1.,0.,0.));
#10477=DIRECTION('',(0.,0.,1.));
#10478=DIRECTION('',(-1.,0.,0.));
#10479=DIRECTION('',(0.,0.,1.));
#10480=DIRECTION('',(-1.,0.,0.));
#10481=DIRECTION('',(0.,0.,1.));
#10482=DIRECTION('',(-1.,0.,0.));
#10483=DIRECTION('',(0.,0.,1.));
#10484=DIRECTION('',(-1.,0.,0.));
#10485=DIRECTION('',(0.,0.,1.));
#10486=DIRECTION('',(-1.,1.1377082542873E-17,-4.88125653654854E-19));
#10487=DIRECTION('',(-1.1377082542873E-17,-1.,0.));
#10488=DIRECTION('',(1.,-1.27684531196004E-12,-3.07678549182519E-17));
#10489=DIRECTION('',(1.27684531196004E-12,1.,0.));
#10490=DIRECTION('',(-1.,0.,0.));
#10491=DIRECTION('',(0.,0.,1.));
#10492=DIRECTION('',(-1.,0.,0.));
#10493=DIRECTION('',(0.,0.,1.));
#10494=DIRECTION('',(-1.,0.,0.));
#10495=DIRECTION('',(0.,0.,1.));
#10496=DIRECTION('',(-1.,0.,0.));
#10497=DIRECTION('',(0.,0.,1.));
#10498=DIRECTION('',(-1.,0.,0.));
#10499=DIRECTION('',(0.,0.,1.));
#10500=DIRECTION('',(-1.,0.,0.));
#10501=DIRECTION('',(0.,0.,1.));
#10502=DIRECTION('',(-1.,0.,0.));
#10503=DIRECTION('',(0.,0.,1.));
#10504=DIRECTION('',(-1.,0.,0.));
#10505=DIRECTION('',(0.,0.,1.));
#10506=DIRECTION('',(-1.,0.,0.));
#10507=DIRECTION('',(0.,0.,1.));
#10508=DIRECTION('',(-1.,0.,0.));
#10509=DIRECTION('',(0.,0.,1.));
#10510=DIRECTION('',(-1.,0.,0.));
#10511=DIRECTION('',(0.,0.,1.));
#10512=DIRECTION('',(-1.,0.,0.));
#10513=DIRECTION('',(0.,0.,1.));
#10514=DIRECTION('',(-1.,0.,0.));
#10515=DIRECTION('',(0.,0.,1.));
#10516=DIRECTION('',(-1.,0.,0.));
#10517=DIRECTION('',(0.,0.,1.));
#10518=DIRECTION('',(-1.,0.,0.));
#10519=DIRECTION('',(0.,0.,1.));
#10520=DIRECTION('',(-1.,0.,0.));
#10521=DIRECTION('',(0.,0.,1.));
#10522=DIRECTION('',(-1.,0.,0.));
#10523=DIRECTION('',(0.,0.,1.));
#10524=DIRECTION('',(-1.,0.,0.));
#10525=DIRECTION('',(0.,0.,1.));
#10526=DIRECTION('',(-1.,0.,0.));
#10527=DIRECTION('',(0.,0.,1.));
#10528=DIRECTION('',(-1.,0.,0.));
#10529=DIRECTION('',(0.,0.,1.));
#10530=DIRECTION('',(-1.,0.,0.));
#10531=DIRECTION('',(0.,0.,1.));
#10532=DIRECTION('',(-1.,0.,0.));
#10533=DIRECTION('',(0.,0.,1.));
#10534=DIRECTION('',(-1.,0.,0.));
#10535=DIRECTION('',(0.,0.,1.));
#10536=DIRECTION('',(-1.,0.,0.));
#10537=DIRECTION('',(0.,0.,1.));
#10538=DIRECTION('',(-1.,0.,0.));
#10539=DIRECTION('',(0.,0.,1.));
#10540=DIRECTION('',(-1.,0.,0.));
#10541=DIRECTION('',(0.,0.,1.));
#10542=DIRECTION('',(-1.,0.,0.));
#10543=DIRECTION('',(0.,0.,1.));
#10544=DIRECTION('',(-1.,0.,0.));
#10545=DIRECTION('',(0.,0.,1.));
#10546=DIRECTION('',(-1.,0.,0.));
#10547=DIRECTION('',(0.,0.,1.));
#10548=DIRECTION('',(1.,0.,0.));
#10549=DIRECTION('',(0.,0.,-1.));
#10550=DIRECTION('',(1.,0.,0.));
#10551=DIRECTION('',(0.,0.,-1.));
#10552=DIRECTION('',(1.,0.,0.));
#10553=DIRECTION('',(0.,0.,-1.));
#10554=DIRECTION('',(1.,0.,0.));
#10555=DIRECTION('',(0.,0.,-1.));
#10556=DIRECTION('',(1.,0.,0.));
#10557=DIRECTION('',(0.,0.,-1.));
#10558=DIRECTION('',(1.,0.,0.));
#10559=DIRECTION('',(0.,0.,-1.));
#10560=DIRECTION('',(1.,0.,0.));
#10561=DIRECTION('',(0.,0.,-1.));
#10562=DIRECTION('',(1.,0.,0.));
#10563=DIRECTION('',(0.,0.,-1.));
#10564=DIRECTION('',(1.,0.,0.));
#10565=DIRECTION('',(0.,0.,-1.));
#10566=DIRECTION('',(1.,0.,0.));
#10567=DIRECTION('',(0.,0.,-1.));
#10568=DIRECTION('',(1.,0.,0.));
#10569=DIRECTION('',(0.,0.,-1.));
#10570=DIRECTION('',(1.,0.,0.));
#10571=DIRECTION('',(0.,0.,-1.));
#10572=DIRECTION('',(1.,0.,0.));
#10573=DIRECTION('',(0.,0.,-1.));
#10574=DIRECTION('',(1.,0.,0.));
#10575=DIRECTION('',(0.,0.,-1.));
#10576=DIRECTION('',(1.,0.,0.));
#10577=DIRECTION('',(0.,0.,-1.));
#10578=DIRECTION('',(1.,0.,0.));
#10579=DIRECTION('',(0.,0.,-1.));
#10580=DIRECTION('',(1.,0.,0.));
#10581=DIRECTION('',(0.,0.,-1.));
#10582=DIRECTION('',(1.,0.,0.));
#10583=DIRECTION('',(0.,0.,-1.));
#10584=DIRECTION('',(-1.,0.,0.));
#10585=DIRECTION('',(0.,0.,1.));
#10586=DIRECTION('',(-1.,0.,0.));
#10587=DIRECTION('',(0.,0.,1.));
#10588=DIRECTION('',(-1.,0.,0.));
#10589=DIRECTION('',(0.,0.,1.));
#10590=DIRECTION('',(-1.,0.,0.));
#10591=DIRECTION('',(0.,0.,1.));
#10592=DIRECTION('',(-1.,0.,0.));
#10593=DIRECTION('',(0.,0.,1.));
#10594=DIRECTION('',(-1.,0.,0.));
#10595=DIRECTION('',(0.,0.,1.));
#10596=DIRECTION('',(-1.,0.,0.));
#10597=DIRECTION('',(0.,0.,1.));
#10598=DIRECTION('',(-1.,0.,0.));
#10599=DIRECTION('',(0.,0.,1.));
#10600=DIRECTION('',(-1.,0.,0.));
#10601=DIRECTION('',(0.,0.,1.));
#10602=DIRECTION('',(-1.,0.,0.));
#10603=DIRECTION('',(0.,0.,1.));
#10604=DIRECTION('',(-1.,0.,0.));
#10605=DIRECTION('',(0.,0.,1.));
#10606=DIRECTION('',(-1.,0.,0.));
#10607=DIRECTION('',(0.,0.,1.));
#10608=DIRECTION('',(-1.,0.,0.));
#10609=DIRECTION('',(0.,0.,1.));
#10610=DIRECTION('',(-1.,0.,0.));
#10611=DIRECTION('',(0.,0.,1.));
#10612=DIRECTION('',(-1.,0.,0.));
#10613=DIRECTION('',(0.,0.,1.));
#10614=DIRECTION('',(-1.,0.,0.));
#10615=DIRECTION('',(0.,0.,1.));
#10616=DIRECTION('',(-1.,0.,0.));
#10617=DIRECTION('',(0.,0.,1.));
#10618=DIRECTION('',(-1.,0.,0.));
#10619=DIRECTION('',(0.,0.,1.));
#10620=DIRECTION('',(-1.,0.,0.));
#10621=DIRECTION('',(0.,0.,1.));
#10622=DIRECTION('',(-1.,0.,0.));
#10623=DIRECTION('',(0.,0.,1.));
#10624=DIRECTION('',(-1.,0.,0.));
#10625=DIRECTION('',(0.,0.,1.));
#10626=DIRECTION('',(-1.,0.,0.));
#10627=DIRECTION('',(0.,0.,1.));
#10628=DIRECTION('',(-1.,0.,0.));
#10629=DIRECTION('',(0.,0.,1.));
#10630=DIRECTION('',(-1.,0.,0.));
#10631=DIRECTION('',(0.,0.,1.));
#10632=DIRECTION('',(-1.,0.,0.));
#10633=DIRECTION('',(0.,0.,1.));
#10634=DIRECTION('',(-1.,0.,0.));
#10635=DIRECTION('',(0.,0.,1.));
#10636=DIRECTION('',(-1.,0.,0.));
#10637=DIRECTION('',(0.,0.,1.));
#10638=DIRECTION('',(-1.,0.,0.));
#10639=DIRECTION('',(0.,0.,1.));
#10640=DIRECTION('',(-1.,0.,0.));
#10641=DIRECTION('',(0.,0.,1.));
#10642=DIRECTION('',(-1.,0.,0.));
#10643=DIRECTION('',(0.,0.,1.));
#10644=DIRECTION('',(-1.,0.,0.));
#10645=DIRECTION('',(0.,0.,1.));
#10646=DIRECTION('',(-1.,0.,0.));
#10647=DIRECTION('',(0.,0.,1.));
#10648=DIRECTION('',(1.,3.14873594454048E-12,1.4723392451601E-16));
#10649=DIRECTION('',(-3.14873594454048E-12,1.,0.));
#10650=DIRECTION('',(1.,-3.14875882929539E-12,-1.47379671248562E-16));
#10651=DIRECTION('',(3.14875882929539E-12,1.,0.));
#10652=DIRECTION('',(1.,-1.30292001398524E-17,1.10016012708286E-17));
#10653=DIRECTION('',(1.30292001398524E-17,1.,0.));
#10654=DIRECTION('',(1.,1.276699066795E-12,-1.73643216677854E-17));
#10655=DIRECTION('',(-1.276699066795E-12,1.,0.));
#10656=DIRECTION('',(1.,-3.40640980091026E-12,4.52734012877115E-17));
#10657=DIRECTION('',(3.40640980091026E-12,1.,0.));
#10658=DIRECTION('',(-1.,0.,0.));
#10659=DIRECTION('',(0.,0.,1.));
#10660=DIRECTION('',(-1.,0.,0.));
#10661=DIRECTION('',(0.,0.,1.));
#10662=DIRECTION('',(-1.,0.,0.));
#10663=DIRECTION('',(0.,0.,1.));
#10664=DIRECTION('',(-1.,0.,0.));
#10665=DIRECTION('',(0.,0.,1.));
#10666=DIRECTION('',(-1.,0.,0.));
#10667=DIRECTION('',(0.,0.,1.));
#10668=DIRECTION('',(-1.,0.,0.));
#10669=DIRECTION('',(0.,0.,1.));
#10670=DIRECTION('',(-1.,0.,0.));
#10671=DIRECTION('',(0.,0.,1.));
#10672=DIRECTION('',(-1.,0.,0.));
#10673=DIRECTION('',(0.,0.,1.));
#10674=DIRECTION('',(-1.,0.,0.));
#10675=DIRECTION('',(0.,0.,1.));
#10676=DIRECTION('',(-1.,0.,0.));
#10677=DIRECTION('',(0.,0.,1.));
#10678=DIRECTION('',(-1.,0.,0.));
#10679=DIRECTION('',(0.,0.,1.));
#10680=DIRECTION('',(-1.,0.,0.));
#10681=DIRECTION('',(0.,0.,1.));
#10682=DIRECTION('',(-1.,0.,0.));
#10683=DIRECTION('',(0.,0.,1.));
#10684=DIRECTION('',(-1.,0.,0.));
#10685=DIRECTION('',(0.,0.,1.));
#10686=DIRECTION('',(-1.,0.,0.));
#10687=DIRECTION('',(0.,0.,1.));
#10688=DIRECTION('',(-1.,0.,0.));
#10689=DIRECTION('',(0.,0.,1.));
#10690=DIRECTION('',(-1.,0.,0.));
#10691=DIRECTION('',(0.,0.,1.));
#10692=DIRECTION('',(-1.,0.,0.));
#10693=DIRECTION('',(0.,0.,1.));
#10694=DIRECTION('',(1.,0.,0.));
#10695=DIRECTION('',(0.,0.,-1.));
#10696=DIRECTION('',(1.,0.,0.));
#10697=DIRECTION('',(0.,0.,-1.));
#10698=DIRECTION('',(1.,0.,0.));
#10699=DIRECTION('',(0.,0.,-1.));
#10700=DIRECTION('',(1.,0.,0.));
#10701=DIRECTION('',(0.,0.,-1.));
#10702=DIRECTION('',(1.,0.,0.));
#10703=DIRECTION('',(0.,0.,-1.));
#10704=DIRECTION('',(1.,0.,0.));
#10705=DIRECTION('',(0.,0.,-1.));
#10706=DIRECTION('',(1.,0.,0.));
#10707=DIRECTION('',(0.,0.,-1.));
#10708=DIRECTION('',(1.,0.,0.));
#10709=DIRECTION('',(0.,0.,-1.));
#10710=DIRECTION('',(1.,0.,0.));
#10711=DIRECTION('',(0.,0.,-1.));
#10712=DIRECTION('',(1.,0.,0.));
#10713=DIRECTION('',(0.,0.,-1.));
#10714=DIRECTION('',(1.,0.,0.));
#10715=DIRECTION('',(0.,0.,-1.));
#10716=DIRECTION('',(1.,0.,0.));
#10717=DIRECTION('',(0.,0.,-1.));
#10718=DIRECTION('',(1.,0.,0.));
#10719=DIRECTION('',(0.,0.,-1.));
#10720=DIRECTION('',(1.,0.,0.));
#10721=DIRECTION('',(0.,0.,-1.));
#10722=DIRECTION('',(1.,0.,0.));
#10723=DIRECTION('',(0.,0.,-1.));
#10724=DIRECTION('',(1.,0.,0.));
#10725=DIRECTION('',(0.,0.,-1.));
#10726=DIRECTION('',(1.,0.,0.));
#10727=DIRECTION('',(0.,0.,-1.));
#10728=DIRECTION('',(1.,0.,0.));
#10729=DIRECTION('',(0.,0.,-1.));
#10730=DIRECTION('',(-1.49022658150495E-16,0.707106781186547,0.707106781186548));
#10731=DIRECTION('',(0.,-0.707106781186548,0.707106781186547));
#10732=DIRECTION('',(1.,0.,0.));
#10733=DIRECTION('',(0.,0.,-1.));
#10734=DIRECTION('',(1.,0.,0.));
#10735=DIRECTION('',(0.,0.,-1.));
#10736=DIRECTION('',(1.,0.,0.));
#10737=DIRECTION('',(0.,0.,-1.));
#10738=DIRECTION('',(1.,0.,0.));
#10739=DIRECTION('',(0.,0.,-1.));
#10740=DIRECTION('',(1.,0.,0.));
#10741=DIRECTION('',(0.,0.,-1.));
#10742=DIRECTION('',(1.,0.,0.));
#10743=DIRECTION('',(0.,0.,-1.));
#10744=DIRECTION('',(1.,0.,0.));
#10745=DIRECTION('',(0.,0.,-1.));
#10746=DIRECTION('',(1.,0.,0.));
#10747=DIRECTION('',(0.,0.,-1.));
#10748=DIRECTION('',(1.,0.,0.));
#10749=DIRECTION('',(0.,0.,-1.));
#10750=DIRECTION('',(1.,0.,0.));
#10751=DIRECTION('',(0.,0.,-1.));
#10752=DIRECTION('',(1.,0.,0.));
#10753=DIRECTION('',(0.,0.,-1.));
#10754=DIRECTION('',(1.,0.,0.));
#10755=DIRECTION('',(0.,0.,-1.));
#10756=DIRECTION('',(1.,0.,0.));
#10757=DIRECTION('',(0.,0.,-1.));
#10758=DIRECTION('',(1.,0.,0.));
#10759=DIRECTION('',(0.,0.,-1.));
#10760=DIRECTION('',(1.,0.,0.));
#10761=DIRECTION('',(0.,0.,-1.));
#10762=DIRECTION('',(1.,0.,0.));
#10763=DIRECTION('',(0.,0.,-1.));
#10764=DIRECTION('',(1.,0.,0.));
#10765=DIRECTION('',(0.,0.,-1.));
#10766=DIRECTION('',(1.,0.,0.));
#10767=DIRECTION('',(0.,0.,-1.));
#10768=DIRECTION('',(-1.06924232066722E-17,-0.965925826292715,0.258819045088912));
#10769=DIRECTION('',(0.,-0.258819045088912,-0.965925826292715));
#10770=DIRECTION('',(-1.,0.,0.));
#10771=DIRECTION('',(0.,0.,1.));
#10772=DIRECTION('',(-1.,0.,0.));
#10773=DIRECTION('',(0.,0.,1.));
#10774=DIRECTION('',(-1.,0.,0.));
#10775=DIRECTION('',(0.,0.,1.));
#10776=DIRECTION('',(3.82310332191275E-18,-0.258819045142856,-0.965925826278261));
#10777=DIRECTION('',(0.,0.965925826278261,-0.258819045142856));
#10778=DIRECTION('',(-4.22965962259824E-18,-0.258819045142856,0.965925826278261));
#10779=DIRECTION('',(0.,-0.965925826278261,-0.258819045142856));
#10780=DIRECTION('',(-1.,0.,0.));
#10781=DIRECTION('',(0.,0.,1.));
#10782=DIRECTION('',(-1.,0.,0.));
#10783=DIRECTION('',(0.,0.,1.));
#10784=DIRECTION('',(-1.,0.,0.));
#10785=DIRECTION('',(0.,0.,1.));
#10786=DIRECTION('',(3.46708220525981E-18,-0.965925826292715,-0.258819045088912));
#10787=DIRECTION('',(0.,0.258819045088912,-0.965925826292715));
#10788=DIRECTION('',(-1.,0.,0.));
#10789=DIRECTION('',(0.,0.,1.));
#10790=DIRECTION('',(-1.,0.,0.));
#10791=DIRECTION('',(0.,0.,1.));
#10792=DIRECTION('',(-1.,0.,0.));
#10793=DIRECTION('',(0.,0.,1.));
#10794=DIRECTION('',(-1.37281479023486E-16,-0.707106781186547,0.707106781186548));
#10795=DIRECTION('',(0.,-0.707106781186548,-0.707106781186547));
#10796=DIRECTION('',(-1.06924232066722E-17,0.965925826292715,-0.258819045088912));
#10797=DIRECTION('',(0.,0.258819045088912,0.965925826292715));
#10798=DIRECTION('',(-1.,0.,0.));
#10799=DIRECTION('',(0.,0.,1.));
#10800=DIRECTION('',(-1.,0.,0.));
#10801=DIRECTION('',(0.,0.,1.));
#10802=DIRECTION('',(-1.,0.,0.));
#10803=DIRECTION('',(0.,0.,1.));
#10804=DIRECTION('',(3.82310332191275E-18,0.258819045142856,0.965925826278261));
#10805=DIRECTION('',(0.,-0.965925826278261,0.258819045142856));
#10806=DIRECTION('',(-4.22965962259824E-18,0.258819045142856,-0.965925826278261));
#10807=DIRECTION('',(0.,0.965925826278261,0.258819045142856));
#10808=DIRECTION('',(-1.,0.,0.));
#10809=DIRECTION('',(0.,0.,1.));
#10810=DIRECTION('',(-1.,0.,0.));
#10811=DIRECTION('',(0.,0.,1.));
#10812=DIRECTION('',(-1.,0.,0.));
#10813=DIRECTION('',(0.,0.,1.));
#10814=DIRECTION('',(3.46708220525981E-18,0.965925826292715,0.258819045088912));
#10815=DIRECTION('',(0.,-0.258819045088912,0.965925826292715));
#10816=DIRECTION('',(-1.49022658150495E-16,-0.707106781186547,-0.707106781186548));
#10817=DIRECTION('',(0.,0.707106781186548,-0.707106781186547));
#10818=DIRECTION('',(-1.,0.,0.));
#10819=DIRECTION('',(0.,0.,1.));
#10820=DIRECTION('',(-1.,0.,0.));
#10821=DIRECTION('',(0.,0.,1.));
#10822=DIRECTION('',(-1.,0.,0.));
#10823=DIRECTION('',(0.,0.,1.));
#10824=DIRECTION('',(-1.37281479023486E-16,0.707106781186547,-0.707106781186548));
#10825=DIRECTION('',(0.,0.707106781186548,0.707106781186547));
#10826=DIRECTION('',(1.,-1.27684531196004E-12,-3.07678549182519E-17));
#10827=DIRECTION('',(1.27684531196004E-12,1.,0.));
#10828=DIRECTION('',(1.,1.27682242720514E-12,2.98634303535282E-17));
#10829=DIRECTION('',(-1.27682242720514E-12,1.,0.));
#10830=DIRECTION('',(-1.,0.,0.));
#10831=DIRECTION('',(0.,0.,1.));
#10832=DIRECTION('',(-1.,0.,0.));
#10833=DIRECTION('',(0.,0.,1.));
#10834=DIRECTION('',(1.,-3.40640980091026E-12,4.52734012877115E-17));
#10835=DIRECTION('',(3.40640980091026E-12,1.,0.));
#10836=DIRECTION('',(-1.,0.,-2.21547530017009E-16));
#10837=DIRECTION('',(-2.21547530017009E-16,0.,1.));
#10838=DIRECTION('',(1.,1.276699066795E-12,-1.73643216677854E-17));
#10839=DIRECTION('',(-1.276699066795E-12,1.,0.));
#10840=DIRECTION('',(1.,-1.27672195154991E-12,1.17909395293212E-17));
#10841=DIRECTION('',(1.27672195154991E-12,1.,0.));
#10842=DIRECTION('',(-1.,0.,0.));
#10843=DIRECTION('',(0.,0.,1.));
#10844=DIRECTION('',(1.,3.40637471308767E-12,-2.04641749438355E-16));
#10845=DIRECTION('',(-3.40637471308767E-12,1.,0.));
#10846=DIRECTION('',(1.,3.40637471308767E-12,-2.04641749438355E-16));
#10847=DIRECTION('',(-3.40637471308767E-12,1.,0.));
#10848=DIRECTION('',(-1.,0.,-2.21547530017009E-16));
#10849=DIRECTION('',(-2.21547530017009E-16,0.,1.));
#10850=DIRECTION('',(-1.,0.,-2.21547530017009E-16));
#10851=DIRECTION('',(-2.21547530017009E-16,0.,1.));
#10852=DIRECTION('',(1.,-1.3591203195553E-17,3.38801252705614E-16));
#10853=DIRECTION('',(3.38801252705614E-16,0.,-1.));
#10854=DIRECTION('',(-1.,0.,0.));
#10855=DIRECTION('',(0.,0.,1.));
#10856=DIRECTION('',(1.,8.2405080686935E-11,-2.00999949487554E-10));
#10857=DIRECTION('',(-2.00999949487554E-10,0.,-1.));
#10858=DIRECTION('',(-1.,0.,0.));
#10859=DIRECTION('',(0.,0.,1.));
#10860=DIRECTION('',(1.,-8.24036101933253E-11,-2.00996350865422E-10));
#10861=DIRECTION('',(-2.00996350865422E-10,0.,-1.));
#10862=DIRECTION('',(-1.,0.,0.));
#10863=DIRECTION('',(0.,0.,1.));
#10864=DIRECTION('',(1.,-2.76226059390704E-10,9.08894019300185E-12));
#10865=DIRECTION('',(2.76226059390704E-10,1.,0.));
#10866=DIRECTION('',(-1.,0.,0.));
#10867=DIRECTION('',(0.,0.,1.));
#10868=DIRECTION('',(1.,-8.2415399410689E-11,2.0101199886441E-10));
#10869=DIRECTION('',(2.0101199886441E-10,0.,-1.));
#10870=DIRECTION('',(-1.,0.,0.));
#10871=DIRECTION('',(0.,0.,1.));
#10872=DIRECTION('',(1.,8.2377328281477E-11,2.00955368657685E-10));
#10873=DIRECTION('',(2.00955368657685E-10,0.,-1.));
#10874=DIRECTION('',(-1.,0.,0.));
#10875=DIRECTION('',(0.,0.,1.));
#10876=DIRECTION('',(1.,2.29382598029866E-10,3.48009873429896E-15));
#10877=DIRECTION('',(-2.29382598029866E-10,1.,0.));
#10878=DIRECTION('',(1.,-1.7553543294653E-16,2.21353907080645E-11));
#10879=DIRECTION('',(2.21353907080645E-11,0.,-1.));
#10880=DIRECTION('',(1.,-2.27117491928019E-11,-1.42033068007457E-15));
#10881=DIRECTION('',(2.27117491928019E-11,1.,0.));
#10882=DIRECTION('',(1.,2.27106160850224E-11,1.38950894359215E-15));
#10883=DIRECTION('',(-2.27106160850224E-11,1.,0.));
#10884=DIRECTION('',(1.,-3.69789685377355E-16,-2.21363853286448E-11));
#10885=DIRECTION('',(-2.21363853286448E-11,0.,-1.));
#10886=DIRECTION('',(1.,-7.05960696451627E-16,-2.21365946134359E-11));
#10887=DIRECTION('',(-2.21365946134359E-11,0.,-1.));
#10888=DIRECTION('',(1.,-2.27106389697773E-11,-1.43717553673992E-15));
#10889=DIRECTION('',(2.27106389697773E-11,1.,0.));
#10890=DIRECTION('',(1.,2.27103940404174E-11,1.44727788746658E-15));
#10891=DIRECTION('',(-2.27103940404174E-11,1.,0.));
#10892=DIRECTION('',(1.,-2.61658203503867E-15,2.2135315939631E-11));
#10893=DIRECTION('',(2.2135315939631E-11,0.,-1.));
#10894=DIRECTION('',(1.,-2.02663347171933E-11,-4.93824078287254E-17));
#10895=DIRECTION('',(2.02663347171933E-11,1.,0.));
#10896=DIRECTION('',(2.02663118324384E-11,-1.,-1.31076765045751E-12));
#10897=DIRECTION('',(1.,2.02663118324384E-11,0.));
#10898=DIRECTION('',(-1.,0.,-9.35772871761781E-16));
#10899=DIRECTION('',(-9.35772871761781E-16,0.,1.));
#10900=DIRECTION('',(-2.02663118324384E-11,1.,-2.64105976331828E-12));
#10901=DIRECTION('',(-1.,-2.02663118324384E-11,0.));
#10902=DIRECTION('',(1.,2.02663118324384E-11,4.37485396368513E-17));
#10903=DIRECTION('',(-2.02663118324384E-11,1.,0.));
#10904=DIRECTION('',(1.,-2.61658203503867E-15,2.2135315939631E-11));
#10905=DIRECTION('',(2.2135315939631E-11,0.,-1.));
#10906=DIRECTION('',(1.,-2.61658203503867E-15,2.2135315939631E-11));
#10907=DIRECTION('',(2.2135315939631E-11,0.,-1.));
#10908=DIRECTION('',(1.,2.27103940404174E-11,1.44727788746658E-15));
#10909=DIRECTION('',(-2.27103940404174E-11,1.,0.));
#10910=DIRECTION('',(1.,2.27103940404174E-11,1.44727788746658E-15));
#10911=DIRECTION('',(-2.27103940404174E-11,1.,0.));
#10912=DIRECTION('',(1.,-2.27106389697773E-11,-1.43717553673992E-15));
#10913=DIRECTION('',(2.27106389697773E-11,1.,0.));
#10914=DIRECTION('',(1.,-7.05960696451627E-16,-2.21365946134359E-11));
#10915=DIRECTION('',(-2.21365946134359E-11,0.,-1.));
#10916=DIRECTION('',(-1.,0.,0.));
#10917=DIRECTION('',(0.,0.,1.));
#10918=DIRECTION('',(1.,-7.05960696451627E-16,-2.21365946134359E-11));
#10919=DIRECTION('',(-2.21365946134359E-11,0.,-1.));
#10920=DIRECTION('',(1.,-3.69789685377355E-16,-2.21363853286448E-11));
#10921=DIRECTION('',(-2.21363853286448E-11,0.,-1.));
#10922=DIRECTION('',(-1.,0.,0.));
#10923=DIRECTION('',(0.,0.,1.));
#10924=DIRECTION('',(1.,-3.69789685377355E-16,-2.21363853286448E-11));
#10925=DIRECTION('',(-2.21363853286448E-11,0.,-1.));
#10926=DIRECTION('',(1.,2.27106160850224E-11,1.38950894359215E-15));
#10927=DIRECTION('',(-2.27106160850224E-11,1.,0.));
#10928=DIRECTION('',(1.,2.27106160850224E-11,1.38950894359215E-15));
#10929=DIRECTION('',(-2.27106160850224E-11,1.,0.));
#10930=DIRECTION('',(1.,-2.27117491928019E-11,-1.42033068007457E-15));
#10931=DIRECTION('',(2.27117491928019E-11,1.,0.));
#10932=DIRECTION('',(1.,-2.27117491928019E-11,-1.42033068007457E-15));
#10933=DIRECTION('',(2.27117491928019E-11,1.,0.));
#10934=DIRECTION('',(1.,-1.7553543294653E-16,2.21353907080645E-11));
#10935=DIRECTION('',(2.21353907080645E-11,0.,-1.));
#10936=DIRECTION('',(1.,-1.7553543294653E-16,2.21353907080645E-11));
#10937=DIRECTION('',(2.21353907080645E-11,0.,-1.));
#10938=DIRECTION('',(-3.57254169227789E-17,0.965925826285055,0.258819045117498));
#10939=DIRECTION('',(0.,-0.258819045117498,0.965925826285055));
#10940=DIRECTION('',(1.,8.2405080686935E-11,-2.00999949487554E-10));
#10941=DIRECTION('',(-2.00999949487554E-10,0.,-1.));
#10942=DIRECTION('',(-4.02472961092684E-18,-0.707106781124562,-0.707106781248533));
#10943=DIRECTION('',(0.,0.707106781248533,-0.707106781124562));
#10944=DIRECTION('',(-1.,0.,0.));
#10945=DIRECTION('',(0.,0.,1.));
#10946=DIRECTION('',(-1.17645942476586E-17,0.707106781124562,-0.707106781248533));
#10947=DIRECTION('',(0.,0.707106781248533,0.707106781124562));
#10948=DIRECTION('',(1.,-8.24036101933253E-11,-2.00996350865422E-10));
#10949=DIRECTION('',(-2.00996350865422E-10,0.,-1.));
#10950=DIRECTION('',(-3.26901987961688E-17,-0.965925826285055,0.258819045117498));
#10951=DIRECTION('',(0.,-0.258819045117498,-0.965925826285055));
#10952=DIRECTION('',(-1.,0.,0.));
#10953=DIRECTION('',(0.,0.,1.));
#10954=DIRECTION('',(0.,0.965925826289012,-0.258819045102731));
#10955=DIRECTION('',(0.,0.258819045102731,0.965925826289012));
#10956=DIRECTION('',(0.,0.965925826289012,-0.258819045102731));
#10957=DIRECTION('',(0.,0.258819045102731,0.965925826289012));
#10958=DIRECTION('',(1.,-2.76226059390704E-10,9.08894019300185E-12));
#10959=DIRECTION('',(2.76226059390704E-10,1.,0.));
#10960=DIRECTION('',(3.50383095897164E-11,0.0940884775756427,-0.995563839433463));
#10961=DIRECTION('',(0.,0.995563839433463,0.0940884775756427));
#10962=DIRECTION('',(1.,-2.76226059390704E-10,9.08894019300185E-12));
#10963=DIRECTION('',(2.76226059390704E-10,1.,0.));
#10964=DIRECTION('',(5.40788131399233E-18,-0.258819045117497,0.965925826285055));
#10965=DIRECTION('',(0.,-0.965925826285055,-0.258819045117497));
#10966=DIRECTION('',(-1.,0.,0.));
#10967=DIRECTION('',(0.,0.,1.));
#10968=DIRECTION('',(-3.57254169227789E-17,-0.965925826285055,-0.258819045117498));
#10969=DIRECTION('',(0.,0.258819045117498,-0.965925826285055));
#10970=DIRECTION('',(1.,-8.2415399410689E-11,2.0101199886441E-10));
#10971=DIRECTION('',(2.0101199886441E-10,0.,-1.));
#10972=DIRECTION('',(-4.02472961092684E-18,0.707106781124562,0.707106781248533));
#10973=DIRECTION('',(0.,-0.707106781248533,0.707106781124562));
#10974=DIRECTION('',(-1.,0.,0.));
#10975=DIRECTION('',(0.,0.,1.));
#10976=DIRECTION('',(-1.17645942476586E-17,-0.707106781124562,0.707106781248533));
#10977=DIRECTION('',(0.,-0.707106781248533,-0.707106781124562));
#10978=DIRECTION('',(1.,8.2377328281477E-11,2.00955368657685E-10));
#10979=DIRECTION('',(2.00955368657685E-10,0.,-1.));
#10980=DIRECTION('',(-3.26901987961688E-17,0.965925826285055,-0.258819045117498));
#10981=DIRECTION('',(0.,0.258819045117498,0.965925826285055));
#10982=DIRECTION('',(-1.,0.,0.));
#10983=DIRECTION('',(0.,0.,1.));
#10984=DIRECTION('',(-3.65658732528797E-18,0.258819045117497,0.965925826285055));
#10985=DIRECTION('',(0.,-0.965925826285055,0.258819045117497));
#10986=DIRECTION('',(1.,2.29382598029866E-10,3.48009873429896E-15));
#10987=DIRECTION('',(-2.29382598029866E-10,1.,0.));
#10988=DIRECTION('',(5.40788131399233E-18,0.258819045117497,-0.965925826285055));
#10989=DIRECTION('',(0.,0.965925826285055,0.258819045117497));
#10990=DIRECTION('',(-1.,0.,0.));
#10991=DIRECTION('',(0.,0.,1.));
#10992=DIRECTION('',(-1.,0.,-9.35772871761781E-16));
#10993=DIRECTION('',(-9.35772871761781E-16,0.,1.));
#10994=DIRECTION('',(-1.,0.,-9.35772871761781E-16));
#10995=DIRECTION('',(-9.35772871761781E-16,0.,1.));
#10996=DIRECTION('',(-1.,0.,-9.35772871761781E-16));
#10997=DIRECTION('',(-9.35772871761781E-16,0.,1.));
#10998=DIRECTION('',(-2.24403093282293E-19,-0.258819045117497,-0.965925826285055));
#10999=DIRECTION('',(0.,0.965925826285055,-0.258819045117497));
#11000=DIRECTION('',(-1.,0.,-9.35772871761781E-16));
#11001=DIRECTION('',(-9.35772871761781E-16,0.,1.));
#11002=DIRECTION('',(-1.,0.,-9.35772871761781E-16));
#11003=DIRECTION('',(-9.35772871761781E-16,0.,1.));
#11004=DIRECTION('',(-1.,0.,-9.35772871761781E-16));
#11005=DIRECTION('',(-9.35772871761781E-16,0.,1.));
#11006=DIRECTION('',(-1.,0.,-9.35772871761781E-16));
#11007=DIRECTION('',(-9.35772871761781E-16,0.,1.));
#11008=DIRECTION('',(-1.,0.,0.));
#11009=DIRECTION('',(0.,0.,1.));
#11010=DIRECTION('',(-1.,0.,0.));
#11011=DIRECTION('',(0.,0.,1.));
#11012=DIRECTION('',(-1.,0.,0.));
#11013=DIRECTION('',(0.,0.,1.));
#11014=DIRECTION('',(-1.,0.,0.));
#11015=DIRECTION('',(0.,0.,1.));
#11016=DIRECTION('',(-1.,0.,0.));
#11017=DIRECTION('',(0.,0.,1.));
#11018=DIRECTION('',(-1.,0.,0.));
#11019=DIRECTION('',(0.,0.,1.));
#11020=DIRECTION('',(-1.,0.,0.));
#11021=DIRECTION('',(0.,0.,1.));
#11022=DIRECTION('',(-1.,0.,0.));
#11023=DIRECTION('',(0.,0.,1.));
#11024=DIRECTION('',(-1.,0.,0.));
#11025=DIRECTION('',(0.,0.,1.));
#11026=DIRECTION('',(-1.,0.,0.));
#11027=DIRECTION('',(0.,0.,1.));
#11028=DIRECTION('',(-1.,0.,0.));
#11029=DIRECTION('',(0.,0.,1.));
#11030=DIRECTION('',(-1.,0.,0.));
#11031=DIRECTION('',(0.,0.,1.));
#11032=DIRECTION('',(-1.,0.,0.));
#11033=DIRECTION('',(0.,0.,1.));
#11034=DIRECTION('',(-1.,0.,0.));
#11035=DIRECTION('',(0.,0.,1.));
#11036=DIRECTION('',(-1.,0.,0.));
#11037=DIRECTION('',(0.,0.,1.));
#11038=DIRECTION('',(-1.,0.,0.));
#11039=DIRECTION('',(0.,0.,1.));
#11040=DIRECTION('',(-1.,0.,0.));
#11041=DIRECTION('',(0.,0.,1.));
#11042=DIRECTION('',(-1.,0.,0.));
#11043=DIRECTION('',(0.,0.,1.));
#11044=DIRECTION('',(-1.,0.,0.));
#11045=DIRECTION('',(0.,0.,1.));
#11046=DIRECTION('',(-1.,0.,0.));
#11047=DIRECTION('',(0.,0.,1.));
#11048=DIRECTION('',(-1.,0.,0.));
#11049=DIRECTION('',(0.,0.,1.));
#11050=DIRECTION('',(-1.,0.,0.));
#11051=DIRECTION('',(0.,0.,1.));
#11052=DIRECTION('',(-1.,0.,0.));
#11053=DIRECTION('',(0.,0.,1.));
#11054=DIRECTION('',(-1.,0.,0.));
#11055=DIRECTION('',(0.,0.,1.));
#11056=DIRECTION('',(-1.,0.,0.));
#11057=DIRECTION('',(0.,0.,1.));
#11058=DIRECTION('',(0.478873989006926,-0.264308029790248,0.83715050501149));
#11059=DIRECTION('',(-1.22147662529582E-10,-0.953600747871024,-0.301074099948542));
#11060=DIRECTION('',(0.497389500059933,-0.242860918363956,0.83283987630369));
#11061=DIRECTION('',(2.92636285103872E-10,0.960015711522541,0.279946126299096));
#11062=DIRECTION('',(1.,5.40052508211967E-11,-5.18934386003978E-11));
#11063=DIRECTION('',(-5.40052508211967E-11,1.,0.));
#11064=DIRECTION('',(0.478873988871033,-0.857147619266543,0.189677783539462));
#11065=DIRECTION('',(6.25680064193633E-10,-0.216062553694835,-0.976379522978061));
#11066=DIRECTION('',(0.497389497976556,-0.842690951126057,0.206096211010516));
#11067=DIRECTION('',(6.54476473210955E-10,0.237567395974056,0.971371058025771));
#11068=DIRECTION('',(1.,6.16564683748603E-10,-4.61139617844463E-15));
#11069=DIRECTION('',(-6.16564683748603E-10,1.,0.));
#11070=DIRECTION('',(-1.,0.,0.));
#11071=DIRECTION('',(0.,0.,1.));
#11072=DIRECTION('',(0.478873986714286,-0.592839591697574,-0.647472720169908));
#11073=DIRECTION('',(1.77654187437559E-9,0.737538191925152,-0.675305423828195));
#11074=DIRECTION('',(0.497389497799453,-0.599830031033446,-0.626743664785871));
#11075=DIRECTION('',(4.46702859689783E-10,-0.72244831369777,0.691424930151675));
#11076=DIRECTION('',(1.,5.40194019363879E-11,5.19075653119709E-11));
#11077=DIRECTION('',(-5.40194019363879E-11,1.,0.));
#11078=DIRECTION('',(0.478873989006939,0.264308029790259,-0.837150505011479));
#11079=DIRECTION('',(-1.22170792175962E-10,0.95360074787102,0.301074099948553));
#11080=DIRECTION('',(0.497389500059914,0.242860918363982,-0.832839876303695));
#11081=DIRECTION('',(2.92636285103876E-10,-0.960015711522533,-0.279946126299123));
#11082=DIRECTION('',(1.,-5.40325554069528E-11,5.19325882603181E-11));
#11083=DIRECTION('',(5.40325554069528E-11,1.,0.));
#11084=DIRECTION('',(0.478873988871033,0.857147619266543,-0.189677783539462));
#11085=DIRECTION('',(6.25680064193633E-10,0.216062553694835,0.976379522978061));
#11086=DIRECTION('',(0.497389497976556,0.842690951126057,-0.206096211010516));
#11087=DIRECTION('',(6.54476473210955E-10,-0.237567395974056,-0.971371058025771));
#11088=DIRECTION('',(1.,-6.16664743242366E-10,3.37120347294801E-15));
#11089=DIRECTION('',(6.16664743242366E-10,1.,0.));
#11090=DIRECTION('',(0.478873986714286,0.592839591697574,0.647472720169908));
#11091=DIRECTION('',(1.77654187437559E-9,-0.737538191925152,0.675305423828195));
#11092=DIRECTION('',(0.497389497799486,0.599830031033462,0.626743664785828));
#11093=DIRECTION('',(4.46656600397107E-10,0.722448313697753,-0.691424930151693));
#11094=DIRECTION('',(1.,-5.40666679703652E-11,-5.19980441369468E-11));
#11095=DIRECTION('',(5.40666679703652E-11,1.,0.));
#11096=DIRECTION('',(0.,0.,-1.));
#11097=DIRECTION('',(-4.44089209850063E-16,1.,0.));
#11098=CARTESIAN_POINT('',(0.,0.,0.));
#11099=CARTESIAN_POINT('',(-0.0285,0.,0.));
#11100=CARTESIAN_POINT('',(0.0175,0.,0.));
#11101=CARTESIAN_POINT('',(0.0175,0.,-0.0115));
#11102=CARTESIAN_POINT('',(-0.0285,0.,0.));
#11103=CARTESIAN_POINT('',(-0.0285,0.,-0.0115));
#11104=CARTESIAN_POINT('',(0.0175,1.39645239816133E-18,-5.20417042793042E-19));
#11105=CARTESIAN_POINT('',(0.0175,0.,0.));
#11106=CARTESIAN_POINT('',(0.0175,0.,0.0125));
#11107=CARTESIAN_POINT('',(-0.0285,-1.35308431126191E-18,-3.98986399474666E-19));
#11108=CARTESIAN_POINT('',(-0.0285,0.,0.));
#11109=CARTESIAN_POINT('',(-0.0285,0.,0.016));
#11110=CARTESIAN_POINT('',(-0.034017463007,0.,0.));
#11111=CARTESIAN_POINT('',(0.016499999985,0.,0.));
#11112=CARTESIAN_POINT('',(0.0164999999925,-0.0124599357945358,0.00099999999823281));
#11113=CARTESIAN_POINT('',(0.0164999998675,-0.012459935929733,-0.00100000000090912));
#11114=CARTESIAN_POINT('',(-0.01749999975,-0.0124599357942312,-0.00100000000181829));
#11115=CARTESIAN_POINT('',(-0.00616666658833333,-0.0124599357942312,-0.00100000000181829));
#11116=CARTESIAN_POINT('',(0.00516666657333334,-0.0124599357942312,-0.00100000000181829));
#11117=CARTESIAN_POINT('',(0.016499999735,-0.0124599357942312,-0.00100000000181829));
#11118=CARTESIAN_POINT('',(-0.0175,-0.0124599357941791,-0.00100000000246662));
#11119=CARTESIAN_POINT('',(-0.0175,0.,0.));
#11120=CARTESIAN_POINT('',(-0.0174999998750001,-0.0121591202350319,-0.0028992754281216));
#11121=CARTESIAN_POINT('',(0.016499999735,-0.0121591201246591,-0.00289927539121607));
#11122=CARTESIAN_POINT('',(0.00516666657333334,-0.0121591201246591,-0.00289927539121607));
#11123=CARTESIAN_POINT('',(-0.00616666658833333,-0.0121591201246591,-0.00289927539121607));
#11124=CARTESIAN_POINT('',(-0.01749999975,-0.0121591201246591,-0.00289927539121607));
#11125=CARTESIAN_POINT('',(0.0164999999925,-0.012159120124003,-0.00289927539363961));
#11126=CARTESIAN_POINT('',(0.016499999985,0.,0.));
#11127=CARTESIAN_POINT('',(0.0164999998675,-0.0115410862648032,-0.00480138846587923));
#11128=CARTESIAN_POINT('',(-0.01749999975,-0.0115410861365096,-0.00480138842311952));
#11129=CARTESIAN_POINT('',(-0.00616666658833333,-0.0115410861365096,-0.00480138842311952));
#11130=CARTESIAN_POINT('',(0.00516666657333334,-0.0115410861365096,-0.00480138842311952));
#11131=CARTESIAN_POINT('',(0.016499999735,-0.0115410861365096,-0.00480138842311952));
#11132=CARTESIAN_POINT('',(-0.0175,-0.0115410861354141,-0.00480138842608671));
#11133=CARTESIAN_POINT('',(-0.0175,0.,0.));
#11134=CARTESIAN_POINT('',(-0.0174999998750001,-0.0106680851512765,-0.00651474958006525));
#11135=CARTESIAN_POINT('',(0.016499999735,-0.0106680850555376,-0.00651474951535476));
#11136=CARTESIAN_POINT('',(0.00516666657333334,-0.0106680850555376,-0.00651474951535476));
#11137=CARTESIAN_POINT('',(-0.00616666658833333,-0.0106680850555376,-0.00651474951535476));
#11138=CARTESIAN_POINT('',(-0.01749999975,-0.0106680850555376,-0.00651474951535476));
#11139=CARTESIAN_POINT('',(0.0164999999925,-0.0106680850565945,-0.00651474951411268));
#11140=CARTESIAN_POINT('',(0.016499999985,0.,0.));
#11141=CARTESIAN_POINT('',(0.0164999998675,-0.00949251466237302,-0.00813278358045513));
#11142=CARTESIAN_POINT('',(-0.01749999975,-0.00949251455069876,-0.0081327835028834));
#11143=CARTESIAN_POINT('',(-0.00616666658833333,-0.00949251455069876,-0.0081327835028834));
#11144=CARTESIAN_POINT('',(0.00516666657333334,-0.00949251455069876,-0.0081327835028834));
#11145=CARTESIAN_POINT('',(0.016499999735,-0.00949251455069876,-0.0081327835028834));
#11146=CARTESIAN_POINT('',(-0.0175,-0.00949251455134075,-0.00813278350213407));
#11147=CARTESIAN_POINT('',(-0.0175,0.,0.));
#11148=CARTESIAN_POINT('',(-0.0174999998750001,-0.00813278356681029,-0.00949251464775881));
#11149=CARTESIAN_POINT('',(0.016499999735,-0.00813278349752703,-0.00949251455528787));
#11150=CARTESIAN_POINT('',(0.00516666657333334,-0.00813278349752703,-0.00949251455528787));
#11151=CARTESIAN_POINT('',(-0.00616666658833333,-0.00813278349752703,-0.00949251455528787));
#11152=CARTESIAN_POINT('',(-0.01749999975,-0.00813278349752703,-0.00949251455528787));
#11153=CARTESIAN_POINT('',(0.0164999999925,-0.0081327834971287,-0.00949251455573178));
#11154=CARTESIAN_POINT('',(0.016499999985,0.,0.));
#11155=CARTESIAN_POINT('',(0.0164999998675,-0.00651474958930339,-0.0106680851684153));
#11156=CARTESIAN_POINT('',(-0.01749999975,-0.00651474950933505,-0.0106680850592137));
#11157=CARTESIAN_POINT('',(-0.00616666658833333,-0.00651474950933505,-0.0106680850592137));
#11158=CARTESIAN_POINT('',(0.00516666657333334,-0.00651474950933505,-0.0106680850592137));
#11159=CARTESIAN_POINT('',(0.016499999735,-0.00651474950933505,-0.0106680850592137));
#11160=CARTESIAN_POINT('',(-0.0175,-0.006514749508334,-0.0106680850599212));
#11161=CARTESIAN_POINT('',(-0.0175,0.,0.));
#11162=CARTESIAN_POINT('',(-0.0174999998750001,-0.00480138846316548,-0.0115410862459344));
#11163=CARTESIAN_POINT('',(0.016499999735,-0.00480138842814829,-0.0115410861344175));
#11164=CARTESIAN_POINT('',(0.00516666657333334,-0.00480138842814829,-0.0115410861344175));
#11165=CARTESIAN_POINT('',(-0.00616666658833333,-0.00480138842814829,-0.0115410861344175));
#11166=CARTESIAN_POINT('',(-0.01749999975,-0.00480138842814829,-0.0115410861344175));
#11167=CARTESIAN_POINT('',(0.0164999999925,-0.00480138842564847,-0.0115410861353612));
#11168=CARTESIAN_POINT('',(0.016499999985,0.,0.));
#11169=CARTESIAN_POINT('',(0.0164999998675,-0.00289927543680423,-0.0121591202526653));
#11170=CARTESIAN_POINT('',(-0.01749999975,-0.00289927539651413,-0.0121591201233958));
#11171=CARTESIAN_POINT('',(-0.00616666658833333,-0.00289927539651413,-0.0121591201233958));
#11172=CARTESIAN_POINT('',(0.00516666657333334,-0.00289927539651413,-0.0121591201233958));
#11173=CARTESIAN_POINT('',(0.016499999735,-0.00289927539651413,-0.0121591201233958));
#11174=CARTESIAN_POINT('',(-0.0175,-0.00289927539331615,-0.0121591201243034));
#11175=CARTESIAN_POINT('',(-0.0175,0.,0.));
#11176=CARTESIAN_POINT('',(-0.0174999998750001,-0.000999999997433504,-0.0124599359095369));
#11177=CARTESIAN_POINT('',(0.016499999735,-0.000999999994787424,-0.0124599357947955));
#11178=CARTESIAN_POINT('',(0.00516666657333334,-0.000999999994787424,-0.0124599357947955));
#11179=CARTESIAN_POINT('',(-0.00616666658833333,-0.000999999994787424,-0.0124599357947955));
#11180=CARTESIAN_POINT('',(-0.01749999975,-0.000999999994787424,-0.0124599357947955));
#11181=CARTESIAN_POINT('',(0.0164999999925,-0.000999999995836203,-0.0124599357949205));
#11182=CARTESIAN_POINT('',(0.016499999985,0.,0.));
#11183=CARTESIAN_POINT('',(0.0164999998675,0.00100000000218691,-0.0124599359296304));
#11184=CARTESIAN_POINT('',(-0.01749999975,0.0010000000043738,-0.0124599357940261));
#11185=CARTESIAN_POINT('',(-0.00616666658833333,0.0010000000043738,-0.0124599357940261));
#11186=CARTESIAN_POINT('',(0.00516666657333334,0.0010000000043738,-0.0124599357940261));
#11187=CARTESIAN_POINT('',(0.016499999735,0.0010000000043738,-0.0124599357940261));
#11188=CARTESIAN_POINT('',(-0.0175,0.0010000000037444,-0.0124599357940766));
#11189=CARTESIAN_POINT('',(-0.0175,0.,0.));
#11190=CARTESIAN_POINT('',(-0.0174999998750001,0.00289927542936853,-0.0121591202347346));
#11191=CARTESIAN_POINT('',(0.016499999735,0.00289927539370995,-0.0121591201240644));
#11192=CARTESIAN_POINT('',(0.00516666657333334,0.00289927539370995,-0.0121591201240644));
#11193=CARTESIAN_POINT('',(-0.00616666658833333,0.00289927539370995,-0.0121591201240644));
#11194=CARTESIAN_POINT('',(-0.01749999975,0.00289927539370995,-0.0121591201240644));
#11195=CARTESIAN_POINT('',(0.0164999999925,0.00289927539491823,-0.0121591201238032));
#11196=CARTESIAN_POINT('',(0.016499999985,0.,0.));
#11197=CARTESIAN_POINT('',(0.0164999998674999,0.00480138846706279,-0.0115410862643108));
#11198=CARTESIAN_POINT('',(-0.01749999975,0.00480138842548664,-0.0115410861355248));
#11199=CARTESIAN_POINT('',(-0.00616666658833333,0.00480138842548664,-0.0115410861355248));
#11200=CARTESIAN_POINT('',(0.00516666657333334,0.00480138842548664,-0.0115410861355248));
#11201=CARTESIAN_POINT('',(0.016499999735,0.00480138842548664,-0.0115410861355248));
#11202=CARTESIAN_POINT('',(-0.0175,0.00480138842723857,-0.0115410861348241));
#11203=CARTESIAN_POINT('',(-0.0175,0.,0.));
#11204=CARTESIAN_POINT('',(-0.0174999998750001,0.00651474957582523,-0.0106680851538658));
#11205=CARTESIAN_POINT('',(0.016499999735,0.00651474950687474,-0.0106680850607162));
#11206=CARTESIAN_POINT('',(0.00516666657333334,0.00651474950687474,-0.0106680850607162));
#11207=CARTESIAN_POINT('',(-0.00616666658833333,0.00651474950687474,-0.0106680850607162));
#11208=CARTESIAN_POINT('',(-0.01749999975,0.00651474950687474,-0.0106680850607162));
#11209=CARTESIAN_POINT('',(0.0164999999925,0.00651474950977088,-0.0106680850590437));
#11210=CARTESIAN_POINT('',(0.016499999985,0.,0.));
#11211=CARTESIAN_POINT('',(0.0164999998674999,0.00813278357668235,-0.00949251466560538));
#11212=CARTESIAN_POINT('',(-0.01749999975,0.00813278349533783,-0.00949251455716348));
#11213=CARTESIAN_POINT('',(-0.00616666658833333,0.00813278349533783,-0.00949251455716348));
#11214=CARTESIAN_POINT('',(0.00516666657333334,0.00813278349533783,-0.00949251455716348));
#11215=CARTESIAN_POINT('',(0.016499999735,0.00813278349533783,-0.00949251455716348));
#11216=CARTESIAN_POINT('',(-0.0175,0.00813278349847502,-0.00949251455472967));
#11217=CARTESIAN_POINT('',(-0.0175,0.,0.));
#11218=CARTESIAN_POINT('',(-0.0174999998750001,0.00949251464859284,-0.00813278356583681));
#11219=CARTESIAN_POINT('',(0.016499999735,0.00949251455695593,-0.00813278349558008));
#11220=CARTESIAN_POINT('',(0.00516666657333334,0.00949251455695593,-0.00813278349558008));
#11221=CARTESIAN_POINT('',(-0.00616666658833333,0.00949251455695593,-0.00813278349558008));
#11222=CARTESIAN_POINT('',(-0.01749999975,0.00949251455695593,-0.00813278349558008));
#11223=CARTESIAN_POINT('',(0.0164999999925,0.00949251455664878,-0.0081327834962155));
#11224=CARTESIAN_POINT('',(0.016499999985,0.,0.));
#11225=CARTESIAN_POINT('',(0.0164999998675,0.0106680851690834,-0.00651474958820936));
#11226=CARTESIAN_POINT('',(-0.01749999975,0.0106680850605499,-0.00651474950714699));
#11227=CARTESIAN_POINT('',(-0.00616666658833333,0.0106680850605499,-0.00651474950714699));
#11228=CARTESIAN_POINT('',(0.00516666657333334,0.0106680850605499,-0.00651474950714699));
#11229=CARTESIAN_POINT('',(0.016499999735,0.0106680850605499,-0.00651474950714699));
#11230=CARTESIAN_POINT('',(-0.0175,0.0106680850605893,-0.00651474950723997));
#11231=CARTESIAN_POINT('',(-0.0175,0.,0.));
#11232=CARTESIAN_POINT('',(-0.0174999998750001,0.0115410862464268,-0.00480138846198192));
#11233=CARTESIAN_POINT('',(0.016499999735,0.0115410861354023,-0.00480138842578117));
#11234=CARTESIAN_POINT('',(0.00516666657333334,0.0115410861354023,-0.00480138842578117));
#11235=CARTESIAN_POINT('',(-0.00616666658833333,0.0115410861354023,-0.00480138842578117));
#11236=CARTESIAN_POINT('',(-0.01749999975,0.0115410861354023,-0.00480138842578117));
#11237=CARTESIAN_POINT('',(0.0164999999925,0.0115410861359511,-0.0048013884244966));
#11238=CARTESIAN_POINT('',(0.016499999985,0.,0.));
#11239=CARTESIAN_POINT('',(0.0164999998675,0.0121591202529626,-0.0028992754355573));
#11240=CARTESIAN_POINT('',(-0.01749999975,0.0121591201239904,-0.00289927539402025));
#11241=CARTESIAN_POINT('',(-0.00616666658833333,0.0121591201239904,-0.00289927539402025));
#11242=CARTESIAN_POINT('',(0.00516666657333334,0.0121591201239904,-0.00289927539402025));
#11243=CARTESIAN_POINT('',(0.016499999735,0.0121591201239904,-0.00289927539402025));
#11244=CARTESIAN_POINT('',(-0.0175,0.0121591201245032,-0.00289927539203753));
#11245=CARTESIAN_POINT('',(-0.0175,0.,0.));
#11246=CARTESIAN_POINT('',(-0.0174999998750001,0.0124599359091394,-0.00100000000238569));
#11247=CARTESIAN_POINT('',(0.016499999735,0.0124599357940006,-0.00100000000469178));
#11248=CARTESIAN_POINT('',(0.00516666657333334,0.0124599357940006,-0.00100000000469178));
#11249=CARTESIAN_POINT('',(-0.00616666658833333,0.0124599357940006,-0.00100000000469178));
#11250=CARTESIAN_POINT('',(-0.01749999975,0.0124599357940006,-0.00100000000469178));
#11251=CARTESIAN_POINT('',(0.0164999999925,0.0124599359297427,-0.00100000000078839));
#11252=CARTESIAN_POINT('',(0.016499999985,0.,0.));
#11253=CARTESIAN_POINT('',(0.0164999998675,0.0124599359300279,0.000999999997234729));
#11254=CARTESIAN_POINT('',(-0.01749999975,0.012459935794821,0.000999999994469453));
#11255=CARTESIAN_POINT('',(-0.00616666658833333,0.012459935794821,0.000999999994469453));
#11256=CARTESIAN_POINT('',(0.00516666657333334,0.012459935794821,0.000999999994469453));
#11257=CARTESIAN_POINT('',(0.016499999735,0.012459935794821,0.000999999994469453));
#11258=CARTESIAN_POINT('',(-0.0175,0.012459935794696,0.000999999998792222));
#11259=CARTESIAN_POINT('',(-0.0175,0.,0.));
#11260=CARTESIAN_POINT('',(-0.0174999998750001,0.0121591202344372,0.00289927543061547));
#11261=CARTESIAN_POINT('',(0.016499999735,0.0121591201234698,0.00289927539620384));
#11262=CARTESIAN_POINT('',(0.00516666657333334,0.0121591201234698,0.00289927539620384));
#11263=CARTESIAN_POINT('',(-0.00616666658833333,0.0121591201234698,0.00289927539620384));
#11264=CARTESIAN_POINT('',(-0.01749999975,0.0121591201234698,0.00289927539620384));
#11265=CARTESIAN_POINT('',(0.0164999999925,0.0121591201236034,0.00289927539619686));
#11266=CARTESIAN_POINT('',(0.016499999985,0.,0.));
#11267=CARTESIAN_POINT('',(0.0164999998675,0.0115410862638184,0.00480138846824635));
#11268=CARTESIAN_POINT('',(-0.01749999975,0.01154108613454,0.00480138842785377));
#11269=CARTESIAN_POINT('',(-0.00616666658833333,0.01154108613454,0.00480138842785377));
#11270=CARTESIAN_POINT('',(0.00516666657333334,0.01154108613454,0.00480138842785377));
#11271=CARTESIAN_POINT('',(0.016499999735,0.01154108613454,0.00480138842785377));
#11272=CARTESIAN_POINT('',(-0.0175,0.0115410861343069,0.00480138842841406));
#11273=CARTESIAN_POINT('',(-0.0175,0.,0.));
#11274=CARTESIAN_POINT('',(-0.0174999998750001,0.0106680851531977,0.00651474957691926));
#11275=CARTESIAN_POINT('',(0.016499999735,0.0106680850593799,0.00651474950906283));
#11276=CARTESIAN_POINT('',(0.00516666657333334,0.0106680850593799,0.00651474950906283));
#11277=CARTESIAN_POINT('',(-0.00616666658833333,0.0106680850593799,0.00651474950906283));
#11278=CARTESIAN_POINT('',(-0.01749999975,0.0106680850593799,0.00651474950906283));
#11279=CARTESIAN_POINT('',(0.0164999999925,0.0106680850583756,0.00651474951086491));
#11280=CARTESIAN_POINT('',(0.016499999985,0.,0.));
#11281=CARTESIAN_POINT('',(0.0164999998675,0.00949251466477135,0.00813278357765582));
#11282=CARTESIAN_POINT('',(-0.01749999975,0.0094925145554954,0.0081327834972848));
#11283=CARTESIAN_POINT('',(-0.00616666658833333,0.0094925145554954,0.0081327834972848));
#11284=CARTESIAN_POINT('',(0.00516666657333334,0.0094925145554954,0.0081327834972848));
#11285=CARTESIAN_POINT('',(0.016499999735,0.0094925145554954,0.0081327834972848));
#11286=CARTESIAN_POINT('',(-0.0175,0.00949251455381267,0.00813278349938822));
#11287=CARTESIAN_POINT('',(-0.0175,0.,0.));
#11288=CARTESIAN_POINT('',(-0.0174999998750001,0.0081327835696096,0.00949251464536048));
#11289=CARTESIAN_POINT('',(0.016499999735,0.00813278350312564,0.00949251455049122));
#11290=CARTESIAN_POINT('',(0.00516666657333334,0.00813278350312564,0.00949251455049122));
#11291=CARTESIAN_POINT('',(-0.00616666658833333,0.00813278350312564,0.00949251455049122));
#11292=CARTESIAN_POINT('',(-0.01749999975,0.00813278350312564,0.00949251455049122));
#11293=CARTESIAN_POINT('',(0.0164999999925,0.00813278349987625,0.00949251455326221));
#11294=CARTESIAN_POINT('',(0.016499999985,0.,0.));
#11295=CARTESIAN_POINT('',(0.0164999998675,0.00651474958711533,0.0106680851697515));
#11296=CARTESIAN_POINT('',(-0.01749999975,0.00651474950495892,0.0106680850618861));
#11297=CARTESIAN_POINT('',(-0.00616666658833333,0.00651474950495892,0.0106680850618861));
#11298=CARTESIAN_POINT('',(0.00516666657333334,0.00651474950495892,0.0106680850618861));
#11299=CARTESIAN_POINT('',(0.016499999735,0.00651474950495892,0.0106680850618861));
#11300=CARTESIAN_POINT('',(-0.0175,0.00651474950614593,0.0106680850612574));
#11301=CARTESIAN_POINT('',(-0.0175,0.,0.));
#11302=CARTESIAN_POINT('',(-0.0174999998750001,0.00480138846079837,0.0115410862469192));
#11303=CARTESIAN_POINT('',(0.016499999735,0.00480138842341404,0.0115410861363871));
#11304=CARTESIAN_POINT('',(0.00516666657333334,0.00480138842341404,0.0115410861363871));
#11305=CARTESIAN_POINT('',(-0.00616666658833333,0.00480138842341404,0.0115410861363871));
#11306=CARTESIAN_POINT('',(-0.01749999975,0.00480138842341404,0.0115410861363871));
#11307=CARTESIAN_POINT('',(0.0164999999925,0.00480138842334474,0.011541086136541));
#11308=CARTESIAN_POINT('',(0.016499999985,0.,0.));
#11309=CARTESIAN_POINT('',(0.0164999998675,0.00289927543431036,0.01215912025326));
#11310=CARTESIAN_POINT('',(-0.01749999975,0.00289927539152635,0.0121591201245851));
#11311=CARTESIAN_POINT('',(-0.00616666658833333,0.00289927539152635,0.0121591201245851));
#11312=CARTESIAN_POINT('',(0.00516666657333334,0.00289927539152635,0.0121591201245851));
#11313=CARTESIAN_POINT('',(0.016499999735,0.00289927539152635,0.0121591201245851));
#11314=CARTESIAN_POINT('',(-0.0175,0.00289927539077852,0.0121591201247634));
#11315=CARTESIAN_POINT('',(-0.0175,0.,0.));
#11316=CARTESIAN_POINT('',(-0.0174999998750001,0.0010000000011079,0.012459935909242));
#11317=CARTESIAN_POINT('',(0.016499999735,0.00100000000213619,0.0124599357942057));
#11318=CARTESIAN_POINT('',(0.00516666657333334,0.00100000000213619,0.0124599357942057));
#11319=CARTESIAN_POINT('',(-0.00616666658833333,0.00100000000213619,0.0124599357942057));
#11320=CARTESIAN_POINT('',(-0.01749999975,0.00100000000213619,0.0124599357942057));
#11321=CARTESIAN_POINT('',(0.0164999999925,0.00099999999873186,0.0124599357942903));
#11322=CARTESIAN_POINT('',(0.016499999985,0.,0.));
#11323=CARTESIAN_POINT('',(0.016499999805,-0.000999999998512521,0.0124599359299253));
#11324=CARTESIAN_POINT('',(-0.01749999975,-0.000999999997025032,0.0124599357946159));
#11325=CARTESIAN_POINT('',(-0.00616666658833333,-0.000999999997025032,0.0124599357946159));
#11326=CARTESIAN_POINT('',(0.00516666657333334,-0.000999999997025032,0.0124599357946159));
#11327=CARTESIAN_POINT('',(0.016499999735,-0.000999999997025032,0.0124599357946159));
#11328=CARTESIAN_POINT('',(-0.0175,-0.00100000000007001,0.0124599357944909));
#11329=CARTESIAN_POINT('',(-0.0175,0.,0.));
#11330=CARTESIAN_POINT('',(-0.0174999998750001,-0.00289927543186242,0.0121591202341399));
#11331=CARTESIAN_POINT('',(0.016499999735,-0.00289927539869773,0.0121591201228751));
#11332=CARTESIAN_POINT('',(0.00516666657333334,-0.00289927539869773,0.0121591201228751));
#11333=CARTESIAN_POINT('',(-0.00616666658833333,-0.00289927539869773,0.0121591201228751));
#11334=CARTESIAN_POINT('',(-0.01749999975,-0.00289927539869773,0.0121591201228751));
#11335=CARTESIAN_POINT('',(0.0164999999925,-0.00289927539747549,0.0121591201234037));
#11336=CARTESIAN_POINT('',(0.016499999985,0.,0.));
#11337=CARTESIAN_POINT('',(0.0164999998675,-0.00480138846942991,0.011541086263326));
#11338=CARTESIAN_POINT('',(-0.01749999975,-0.00480138843022089,0.0115410861335552));
#11339=CARTESIAN_POINT('',(-0.00616666658833333,-0.00480138843022089,0.0115410861335552));
#11340=CARTESIAN_POINT('',(0.00516666657333334,-0.00480138843022089,0.0115410861335552));
#11341=CARTESIAN_POINT('',(0.016499999735,-0.00480138843022089,0.0115410861335552));
#11342=CARTESIAN_POINT('',(-0.0175,-0.00480138842959763,0.0115410861338145));
#11343=CARTESIAN_POINT('',(-0.0175,0.,0.));
#11344=CARTESIAN_POINT('',(-0.0174999998750001,-0.00651474957801329,0.0106680851525296));
#11345=CARTESIAN_POINT('',(0.016499999735,-0.00651474951125087,0.0106680850580438));
#11346=CARTESIAN_POINT('',(0.00516666657333334,-0.00651474951125087,0.0106680850580438));
#11347=CARTESIAN_POINT('',(-0.00616666658833333,-0.00651474951125087,0.0106680850580438));
#11348=CARTESIAN_POINT('',(-0.01749999975,-0.00651474951125087,0.0106680850580438));
#11349=CARTESIAN_POINT('',(0.0164999999925,-0.00651474951195894,0.0106680850577075));
#11350=CARTESIAN_POINT('',(0.016499999985,0.,0.));
#11351=CARTESIAN_POINT('',(0.0164999998675,-0.0081327835786293,0.00949251466393732));
#11352=CARTESIAN_POINT('',(-0.01749999975,-0.00813278349923174,0.00949251455382735));
#11353=CARTESIAN_POINT('',(-0.00616666658833333,-0.00813278349923174,0.00949251455382735));
#11354=CARTESIAN_POINT('',(0.00516666657333334,-0.00813278349923174,0.00949251455382735));
#11355=CARTESIAN_POINT('',(0.016499999735,-0.00813278349923174,0.00949251455382735));
#11356=CARTESIAN_POINT('',(-0.0175,-0.00813278350030823,0.00949251455290506));
#11357=CARTESIAN_POINT('',(-0.0175,0.,0.));
#11358=CARTESIAN_POINT('',(-0.0174999998750001,-0.00949251464619451,0.00813278356863612));
#11359=CARTESIAN_POINT('',(0.016499999735,-0.00949251455215928,0.00813278350117869));
#11360=CARTESIAN_POINT('',(0.00516666657333334,-0.00949251455215928,0.00813278350117869));
#11361=CARTESIAN_POINT('',(-0.00616666658833333,-0.00949251455215928,0.00813278350117869));
#11362=CARTESIAN_POINT('',(-0.01749999975,-0.00949251455215928,0.00813278350117869));
#11363=CARTESIAN_POINT('',(0.0164999999925,-0.00949251455409624,0.00813278349890277));
#11364=CARTESIAN_POINT('',(0.016499999985,0.,0.));
#11365=CARTESIAN_POINT('',(0.0164999998675,-0.0106680851671622,0.00651474959135534));
#11366=CARTESIAN_POINT('',(-0.01749999975,-0.0106680850567076,0.00651474951343894));
#11367=CARTESIAN_POINT('',(-0.00616666658833333,-0.0106680850567076,0.00651474951343894));
#11368=CARTESIAN_POINT('',(0.00516666657333334,-0.0106680850567076,0.00651474951343894));
#11369=CARTESIAN_POINT('',(0.016499999735,-0.0106680850567076,0.00651474951343894));
#11370=CARTESIAN_POINT('',(-0.0175,-0.0106680850587356,0.00651474951043495));
#11371=CARTESIAN_POINT('',(-0.0175,0.,0.));
#11372=CARTESIAN_POINT('',(-0.0174999998750001,-0.0115410862474116,0.00480138845961481));
#11373=CARTESIAN_POINT('',(0.016499999735,-0.0115410861373718,0.00480138842104692));
#11374=CARTESIAN_POINT('',(0.00516666657333334,-0.0115410861373718,0.00480138842104692));
#11375=CARTESIAN_POINT('',(-0.00616666658833333,-0.0115410861373718,0.00480138842104692));
#11376=CARTESIAN_POINT('',(-0.01749999975,-0.0115410861373718,0.00480138842104692));
#11377=CARTESIAN_POINT('',(0.0164999999925,-0.0115410861371309,0.00480138842219287));
#11378=CARTESIAN_POINT('',(0.016499999985,0.,0.));
#11379=CARTESIAN_POINT('',(0.0164999998675,-0.0121591202535573,0.00289927543306342));
#11380=CARTESIAN_POINT('',(-0.01749999975,-0.0121591201251797,0.00289927538903248));
#11381=CARTESIAN_POINT('',(-0.00616666658833333,-0.0121591201251797,0.00289927538903248));
#11382=CARTESIAN_POINT('',(0.00516666657333334,-0.0121591201251797,0.00289927538903248));
#11383=CARTESIAN_POINT('',(0.016499999735,-0.0121591201251797,0.00289927538903248));
#11384=CARTESIAN_POINT('',(-0.0175,-0.0121591201250607,0.00289927538953159));
#11385=CARTESIAN_POINT('',(-0.0175,0.,0.));
#11386=CARTESIAN_POINT('',(-0.0174999998750001,-0.0124599359093445,0.000999999999830113));
#11387=CARTESIAN_POINT('',(0.016499999735,-0.0124599357944108,0.000999999999580603));
#11388=CARTESIAN_POINT('',(0.00516666657333334,-0.0124599357944108,0.000999999999580603));
#11389=CARTESIAN_POINT('',(-0.00616666658833333,-0.0124599357944108,0.000999999999580603));
#11390=CARTESIAN_POINT('',(-0.01749999975,-0.0124599357944108,0.000999999999580603));
#11391=CARTESIAN_POINT('',(-0.034017463007,0.,0.));
#11392=CARTESIAN_POINT('',(-0.0215,0.,0.));
#11393=CARTESIAN_POINT('',(-0.0215,0.,0.016));
#11394=CARTESIAN_POINT('',(0.0165,0.012729967897,-1.56125112837913E-19));
#11395=CARTESIAN_POINT('',(0.0165,0.0124599359297427,-0.001));
#11396=CARTESIAN_POINT('',(0.0165,0.012627117751961,-0.001));
#11397=CARTESIAN_POINT('',(0.0165,0.0127942995741793,-0.001));
#11398=CARTESIAN_POINT('',(0.0165,0.0129614813963976,-0.001));
#11399=CARTESIAN_POINT('',(0.016499999875,0.0129614813972715,-0.000999999995286969));
#11400=CARTESIAN_POINT('',(0.0165,0.,0.));
#11401=CARTESIAN_POINT('',(0.0165,0.0129614812809713,0.001));
#11402=CARTESIAN_POINT('',(0.0165,0.0129614812809713,0.001));
#11403=CARTESIAN_POINT('',(0.0165,0.0127942994973235,0.001));
#11404=CARTESIAN_POINT('',(0.0165,0.0126271177136757,0.001));
#11405=CARTESIAN_POINT('',(0.0165,0.0124599359300279,0.001));
#11406=CARTESIAN_POINT('',(-0.0005,0.0127107085955,0.001));
#11407=CARTESIAN_POINT('',(0.0165,0.012961481397,0.001));
#11408=CARTESIAN_POINT('',(0.00550000000333333,0.012961481397,0.001));
#11409=CARTESIAN_POINT('',(-0.00549999999333333,0.012961481397,0.001));
#11410=CARTESIAN_POINT('',(-0.01649999999,0.012961481397,0.001));
#11411=CARTESIAN_POINT('',(-0.016499999995,0.0129614813969079,0.001));
#11412=CARTESIAN_POINT('',(-0.01649999999,0.012961481397,0.001));
#11413=CARTESIAN_POINT('',(-0.0168333333266667,0.012961481397,0.001));
#11414=CARTESIAN_POINT('',(-0.0171666666633333,0.012961481397,0.001));
#11415=CARTESIAN_POINT('',(-0.0175,0.012961481397,0.001));
#11416=CARTESIAN_POINT('',(-0.0175,0.0129614813972181,0.00100000000002654));
#11417=CARTESIAN_POINT('',(-0.0175,0.012961481397,0.001));
#11418=CARTESIAN_POINT('',(-0.0175,0.0127942995293333,0.001));
#11419=CARTESIAN_POINT('',(-0.0175,0.0126271176616667,0.001));
#11420=CARTESIAN_POINT('',(-0.0175,0.012459935794,0.001));
#11421=CARTESIAN_POINT('',(-0.0175,0.014827238428,0.002713045933));
#11422=CARTESIAN_POINT('',(-0.0175000000005,0.,0.));
#11423=CARTESIAN_POINT('',(-0.0175,0.0167636388755286,0.00502298781439511));
#11424=CARTESIAN_POINT('',(-0.0174999998755,0.0174953567318995,0.000403103986062307));
#11425=CARTESIAN_POINT('',(-0.0175,0.0126361183371985,0.00305426150693499));
#11426=CARTESIAN_POINT('',(-0.0175,0.0140119585166962,0.00371050360930785));
#11427=CARTESIAN_POINT('',(-0.0175,0.0153877986961938,0.0043667457116807));
#11428=CARTESIAN_POINT('',(-0.0175,0.0167636388756915,0.00502298781405356));
#11429=CARTESIAN_POINT('',(-0.0175,0.0126361183374657,0.00305426150728999));
#11430=CARTESIAN_POINT('',(-0.0175,0.0121591202349204,0.00289927542912857));
#11431=CARTESIAN_POINT('',(-0.0175,0.0123181196023464,0.00295093745506404));
#11432=CARTESIAN_POINT('',(-0.0175,0.0124771189697725,0.00300259948099951));
#11433=CARTESIAN_POINT('',(-0.0175,0.0126361183371985,0.00305426150693499));
#11434=CARTESIAN_POINT('',(-0.0175,0.0174953567323097,0.000403103989178478));
#11435=CARTESIAN_POINT('',(-0.0175,0.0159840649540913,0.000602069326145522));
#11436=CARTESIAN_POINT('',(-0.0175,0.0144727731758729,0.000801034663112566));
#11437=CARTESIAN_POINT('',(-0.0175,0.0129614813976545,0.00100000000007961));
#11438=CARTESIAN_POINT('',(-0.0005,0.012397619231,0.0029767684505));
#11439=CARTESIAN_POINT('',(-0.0175,0.012636118338,0.003054261508));
#11440=CARTESIAN_POINT('',(-0.0171666666633333,0.012636118338,0.003054261508));
#11441=CARTESIAN_POINT('',(-0.0168333333266667,0.012636118338,0.003054261508));
#11442=CARTESIAN_POINT('',(-0.01649999999,0.012636118338,0.003054261508));
#11443=CARTESIAN_POINT('',(-0.016499999995,0.0126361183378015,0.00305426150790531));
#11444=CARTESIAN_POINT('',(-0.01649999999,0.012636118338,0.003054261508));
#11445=CARTESIAN_POINT('',(-0.00549999999333333,0.012636118338,0.003054261508));
#11446=CARTESIAN_POINT('',(0.00550000000333333,0.012636118338,0.003054261508));
#11447=CARTESIAN_POINT('',(0.0165,0.012636118338,0.003054261508));
#11448=CARTESIAN_POINT('',(0.0165,0.0126361181000306,0.00305426143067905));
#11449=CARTESIAN_POINT('',(0.0165,0.0126361181000306,0.00305426143067905));
#11450=CARTESIAN_POINT('',(0.0165,0.0124771187746871,0.00300259941811937));
#11451=CARTESIAN_POINT('',(0.0165,0.0123181194493435,0.00295093740555969));
#11452=CARTESIAN_POINT('',(0.0165,0.012159120124,0.002899275393));
#11453=CARTESIAN_POINT('',(0.0165,0.0120886022365,0.00392782496649999));
#11454=CARTESIAN_POINT('',(0.0165,0.,0.));
#11455=CARTESIAN_POINT('',(0.0165,0.0120180842387746,0.00495637450404248));
#11456=CARTESIAN_POINT('',(0.0165,0.0120180842388167,0.00495637450391302));
#11457=CARTESIAN_POINT('',(0.0165,0.0118590849139752,0.00490471249153795));
#11458=CARTESIAN_POINT('',(0.0165,0.0117000855891338,0.00485305047916288));
#11459=CARTESIAN_POINT('',(0.0165,0.0115410862642923,0.00480138846678781));
#11460=CARTESIAN_POINT('',(-0.0005,0.011779585242,0.004878881483));
#11461=CARTESIAN_POINT('',(0.0165,0.012018084349,0.00495637454));
#11462=CARTESIAN_POINT('',(0.00550000000333333,0.012018084349,0.00495637454));
#11463=CARTESIAN_POINT('',(-0.00549999999333332,0.012018084349,0.00495637454));
#11464=CARTESIAN_POINT('',(-0.01649999999,0.012018084349,0.00495637454));
#11465=CARTESIAN_POINT('',(-0.016499999995,0.0120180843489919,0.00495637453999739));
#11466=CARTESIAN_POINT('',(-0.01649999999,0.012018084349,0.00495637454));
#11467=CARTESIAN_POINT('',(-0.0168333333266667,0.012018084349,0.00495637454));
#11468=CARTESIAN_POINT('',(-0.0171666666633333,0.012018084349,0.00495637454));
#11469=CARTESIAN_POINT('',(-0.0175,0.012018084349,0.00495637454));
#11470=CARTESIAN_POINT('',(-0.0175,0.0120180843492958,0.00495637454010061));
#11471=CARTESIAN_POINT('',(-0.0175,0.012018084349,0.00495637454));
#11472=CARTESIAN_POINT('',(-0.0175,0.0118590849443333,0.004904712502));
#11473=CARTESIAN_POINT('',(-0.0175,0.0117000855396667,0.004853050464));
#11474=CARTESIAN_POINT('',(-0.0175,0.011541086135,0.004801388426));
#11475=CARTESIAN_POINT('',(-0.0175,0.0135912960505,0.0073793915595));
#11476=CARTESIAN_POINT('',(-0.0175,0.016514507041402,0.00578973722594494));
#11477=CARTESIAN_POINT('',(-0.0175,0.0150156994775638,0.0055119496640639));
#11478=CARTESIAN_POINT('',(-0.0175,0.0135168919137255,0.00523416210218287));
#11479=CARTESIAN_POINT('',(-0.0175,0.0120180843498873,0.00495637454030183));
#11480=CARTESIAN_POINT('',(-0.0174999997505,0.0165145070402477,0.00578973723217286));
#11481=CARTESIAN_POINT('',(-0.0175000000005,0.,0.));
#11482=CARTESIAN_POINT('',(-0.0174999998752501,0.0143909793913725,0.00995739459196203));
#11483=CARTESIAN_POINT('',(-0.0175,0.0110738439744768,0.00680955061903613));
#11484=CARTESIAN_POINT('',(-0.0175,0.0121795557799528,0.00785883194350906));
#11485=CARTESIAN_POINT('',(-0.0175,0.0132852675854288,0.00890811326798199));
#11486=CARTESIAN_POINT('',(-0.0175,0.0143909793909048,0.00995739459245492));
#11487=CARTESIAN_POINT('',(-0.0175,0.0110738439746512,0.00680955061902408));
#11488=CARTESIAN_POINT('',(-0.0175,0.0106680851533433,0.00651474957671889));
#11489=CARTESIAN_POINT('',(-0.0175,0.0108033380937212,0.00661301659082463));
#11490=CARTESIAN_POINT('',(-0.0175,0.010938591034099,0.00671128360493038));
#11491=CARTESIAN_POINT('',(-0.0175,0.0110738439744768,0.00680955061903613));
#11492=CARTESIAN_POINT('',(-0.0005,0.010870964517,0.00666215006449998));
#11493=CARTESIAN_POINT('',(-0.0175,0.011073843975,0.00680955061899999));
#11494=CARTESIAN_POINT('',(-0.0171666666633333,0.011073843975,0.00680955061899999));
#11495=CARTESIAN_POINT('',(-0.0168333333266667,0.011073843975,0.00680955061899999));
#11496=CARTESIAN_POINT('',(-0.01649999999,0.011073843975,0.00680955061899999));
#11497=CARTESIAN_POINT('',(-0.016499999995,0.0110738439747809,0.00680955061879209));
#11498=CARTESIAN_POINT('',(-0.01649999999,0.011073843975,0.00680955061899999));
#11499=CARTESIAN_POINT('',(-0.00549999999333334,0.011073843975,0.00680955061899999));
#11500=CARTESIAN_POINT('',(0.00550000000333334,0.011073843975,0.00680955061899999));
#11501=CARTESIAN_POINT('',(0.0165,0.011073843975,0.00680955061899999));
#11502=CARTESIAN_POINT('',(0.0165,0.011073843772506,0.00680955047187945));
#11503=CARTESIAN_POINT('',(0.0165,0.011073843772506,0.00680955047187945));
#11504=CARTESIAN_POINT('',(0.0165,0.010938590868004,0.0067112834845863));
#11505=CARTESIAN_POINT('',(0.0165,0.010803337963502,0.00661301649729314));
#11506=CARTESIAN_POINT('',(0.0165,0.010668085059,0.00651474950999999));
#11507=CARTESIAN_POINT('',(0.0165,0.0102831792645,0.0074711670585));
#11508=CARTESIAN_POINT('',(0.0165,0.,0.));
#11509=CARTESIAN_POINT('',(0.0165,0.00989827337663452,0.00842758453894735));
#11510=CARTESIAN_POINT('',(0.0165,0.00989827337673848,0.00842758453880426));
#11511=CARTESIAN_POINT('',(0.0165,0.00976302047259451,0.00832931755196802));
#11512=CARTESIAN_POINT('',(0.0165,0.00962776756845054,0.00823105056513178));
#11513=CARTESIAN_POINT('',(0.0165,0.00949251466430657,0.00813278357829554));
#11514=CARTESIAN_POINT('',(-0.0005,0.00969539401200001,0.00828018405299999));
#11515=CARTESIAN_POINT('',(0.0165,0.00989827347000001,0.00842758460699999));
#11516=CARTESIAN_POINT('',(0.00550000000333334,0.00989827347000001,0.00842758460699999));
#11517=CARTESIAN_POINT('',(-0.00549999999333334,0.00989827347000001,0.00842758460699999));
#11518=CARTESIAN_POINT('',(-0.01649999999,0.00989827347000001,0.00842758460699999));
#11519=CARTESIAN_POINT('',(-0.016499999995,0.00989827347007726,0.00842758460705612));
#11520=CARTESIAN_POINT('',(-0.01649999999,0.00989827347000001,0.00842758460699999));
#11521=CARTESIAN_POINT('',(-0.0168333333266667,0.00989827347000001,0.00842758460699999));
#11522=CARTESIAN_POINT('',(-0.0171666666633333,0.00989827347000001,0.00842758460699999));
#11523=CARTESIAN_POINT('',(-0.0175,0.00989827347000001,0.00842758460699999));
#11524=CARTESIAN_POINT('',(-0.0175,0.0098982734697996,0.00842758460672372));
#11525=CARTESIAN_POINT('',(-0.0175,0.00989827347000001,0.00842758460699999));
#11526=CARTESIAN_POINT('',(-0.0175,0.00976302049800001,0.00832931757099999));
#11527=CARTESIAN_POINT('',(-0.0175,0.00962776752600001,0.00823105053499999));
#11528=CARTESIAN_POINT('',(-0.0175,0.00949251455400001,0.00813278349899999));
#11529=CARTESIAN_POINT('',(-0.0175,0.011024942919,0.011024942919));
#11530=CARTESIAN_POINT('',(-0.0175,0.0139171023379207,0.010609630650532));
#11531=CARTESIAN_POINT('',(-0.0175,0.0125774927150801,0.00988228196907837));
#11532=CARTESIAN_POINT('',(-0.0175,0.0112378830922394,0.00915493328762477));
#11533=CARTESIAN_POINT('',(-0.0175,0.00989827346939877,0.00842758460617117));
#11534=CARTESIAN_POINT('',(-0.0174999997505,0.0139171023401316,0.01060963064646));
#11535=CARTESIAN_POINT('',(-0.0175000000005,0.,0.));
#11536=CARTESIAN_POINT('',(-0.0174999998752501,0.010609630582124,0.0139171022078995));
#11537=CARTESIAN_POINT('',(-0.0175,0.00842758460617116,0.00989827346939878));
#11538=CARTESIAN_POINT('',(-0.0175,0.00915493326425888,0.0112378830492048));
#11539=CARTESIAN_POINT('',(-0.0175,0.00988228192234659,0.0125774926290109));
#11540=CARTESIAN_POINT('',(-0.0175,0.0106096305804343,0.0139171022088169));
#11541=CARTESIAN_POINT('',(-0.0175,0.00842758460644744,0.00989827346959919));
#11542=CARTESIAN_POINT('',(-0.0175,0.0081327835680109,0.00949251464652199));
#11543=CARTESIAN_POINT('',(-0.0175,0.00823105058073098,0.00962776758748092));
#11544=CARTESIAN_POINT('',(-0.0175,0.00832931759345107,0.00976302052843985));
#11545=CARTESIAN_POINT('',(-0.0175,0.00842758460617116,0.00989827346939878));
#11546=CARTESIAN_POINT('',(-0.0005,0.00828018405299999,0.009695394012));
#11547=CARTESIAN_POINT('',(-0.0175,0.00842758460699999,0.00989827347000001));
#11548=CARTESIAN_POINT('',(-0.0171666666633333,0.00842758460699999,0.00989827347000001));
#11549=CARTESIAN_POINT('',(-0.0168333333266667,0.00842758460699999,0.00989827347000001));
#11550=CARTESIAN_POINT('',(-0.01649999999,0.00842758460699999,0.00989827347000001));
#11551=CARTESIAN_POINT('',(-0.016499999995,0.00842758460704643,0.00989827347008551));
#11552=CARTESIAN_POINT('',(-0.01649999999,0.00842758460699999,0.00989827347000001));
#11553=CARTESIAN_POINT('',(-0.00549999999333333,0.00842758460699999,0.00989827347000001));
#11554=CARTESIAN_POINT('',(0.00550000000333333,0.00842758460699999,0.00989827347000001));
#11555=CARTESIAN_POINT('',(0.0165,0.00842758460699999,0.00989827347000001));
#11556=CARTESIAN_POINT('',(0.0165,0.00842758446010981,0.00989827326782301));
#11557=CARTESIAN_POINT('',(0.0165,0.00842758446010981,0.00989827326782301));
#11558=CARTESIAN_POINT('',(0.0165,0.0083293174730732,0.00976302036321534));
#11559=CARTESIAN_POINT('',(0.0165,0.0082310504860366,0.00962776745860767));
#11560=CARTESIAN_POINT('',(0.0165,0.00813278349899999,0.009492514554));
#11561=CARTESIAN_POINT('',(0.0165,0.0074711670585,0.0102831792645));
#11562=CARTESIAN_POINT('',(0.0165,0.,0.));
#11563=CARTESIAN_POINT('',(0.0165,0.0068095505505698,0.0110738438809193));
#11564=CARTESIAN_POINT('',(0.0165,0.0068095505505197,0.0110738438809557));
#11565=CARTESIAN_POINT('',(0.0165,0.00671128356354459,0.0109385909766206));
#11566=CARTESIAN_POINT('',(0.0165,0.00661301657656948,0.0108033380722855));
#11567=CARTESIAN_POINT('',(0.0165,0.00651474958959437,0.0106680851679504));
#11568=CARTESIAN_POINT('',(-0.0005,0.00666215006449997,0.010870964517));
#11569=CARTESIAN_POINT('',(0.0165,0.00680955061899998,0.011073843975));
#11570=CARTESIAN_POINT('',(0.00550000000333333,0.00680955061899998,0.011073843975));
#11571=CARTESIAN_POINT('',(-0.00549999999333332,0.00680955061899998,0.011073843975));
#11572=CARTESIAN_POINT('',(-0.01649999999,0.00680955061899998,0.011073843975));
#11573=CARTESIAN_POINT('',(-0.016499999995,0.00680955061882576,0.0110738439747602));
#11574=CARTESIAN_POINT('',(-0.01649999999,0.00680955061899998,0.011073843975));
#11575=CARTESIAN_POINT('',(-0.0168333333266667,0.00680955061899998,0.011073843975));
#11576=CARTESIAN_POINT('',(-0.0171666666633333,0.00680955061899998,0.011073843975));
#11577=CARTESIAN_POINT('',(-0.0175,0.00680955061899998,0.011073843975));
#11578=CARTESIAN_POINT('',(-0.0175,0.00680955061901203,0.0110738439748256));
#11579=CARTESIAN_POINT('',(-0.0175,0.00680955061899998,0.011073843975));
#11580=CARTESIAN_POINT('',(-0.0175,0.00671128358266665,0.010938591003));
#11581=CARTESIAN_POINT('',(-0.0175,0.00661301654633331,0.010803338031));
#11582=CARTESIAN_POINT('',(-0.0175,0.00651474950999998,0.010668085059));
#11583=CARTESIAN_POINT('',(-0.0175,0.0073793915595,0.0135912960505));
#11584=CARTESIAN_POINT('',(-0.0175,0.00995739469288571,0.0143909794967367));
#11585=CARTESIAN_POINT('',(-0.0175,0.00890811333493585,0.0132852676559834));
#11586=CARTESIAN_POINT('',(-0.0175,0.00785883197698599,0.0121795558152301));
#11587=CARTESIAN_POINT('',(-0.0175,0.00680955061903612,0.0110738439744768));
#11588=CARTESIAN_POINT('',(-0.0174999997505,0.00995739468550641,0.0143909795037394));
#11589=CARTESIAN_POINT('',(-0.0175000000005,0.,0.));
#11590=CARTESIAN_POINT('',(-0.0174999998752501,0.00578973719816985,0.0165145068983457));
#11591=CARTESIAN_POINT('',(-0.0175,0.00495637454030183,0.0120180843498873));
#11592=CARTESIAN_POINT('',(-0.0175,0.00523416209333093,0.0135168918659648));
#11593=CARTESIAN_POINT('',(-0.0175,0.00551194964636003,0.0150156993820422));
#11594=CARTESIAN_POINT('',(-0.0175,0.00578973719938913,0.0165145068981197));
#11595=CARTESIAN_POINT('',(-0.0175,0.00495637454020122,0.0120180843495915));
#11596=CARTESIAN_POINT('',(-0.0175,0.00480138846212824,0.0115410862464871));
#11597=CARTESIAN_POINT('',(-0.0175,0.0048530504881861,0.0117000856142871));
#11598=CARTESIAN_POINT('',(-0.0175,0.00490471251424396,0.0118590849820872));
#11599=CARTESIAN_POINT('',(-0.0175,0.00495637454030183,0.0120180843498873));
#11600=CARTESIAN_POINT('',(-0.0005,0.004878881483,0.011779585242));
#11601=CARTESIAN_POINT('',(-0.0175,0.00495637454,0.012018084349));
#11602=CARTESIAN_POINT('',(-0.0171666666633333,0.00495637454,0.012018084349));
#11603=CARTESIAN_POINT('',(-0.0168333333266667,0.00495637454,0.012018084349));
#11604=CARTESIAN_POINT('',(-0.01649999999,0.00495637454,0.012018084349));
#11605=CARTESIAN_POINT('',(-0.016499999995,0.00495637453999843,0.0120180843489915));
#11606=CARTESIAN_POINT('',(-0.01649999999,0.00495637454,0.012018084349));
#11607=CARTESIAN_POINT('',(-0.00549999999333334,0.00495637454,0.012018084349));
#11608=CARTESIAN_POINT('',(0.00550000000333334,0.00495637454,0.012018084349));
#11609=CARTESIAN_POINT('',(0.0165,0.00495637454,0.012018084349));
#11610=CARTESIAN_POINT('',(0.0165,0.00495637446274314,0.0120180841112278));
#11611=CARTESIAN_POINT('',(0.0165,0.00495637446274314,0.0120180841112278));
#11612=CARTESIAN_POINT('',(0.0165,0.00490471245049542,0.0118590847858185));
#11613=CARTESIAN_POINT('',(0.0165,0.00485305043824771,0.0117000854604093));
#11614=CARTESIAN_POINT('',(0.0165,0.004801388426,0.011541086135));
#11615=CARTESIAN_POINT('',(0.0165,0.0039278249665,0.0120886022365));
#11616=CARTESIAN_POINT('',(0.0165,0.,0.));
#11617=CARTESIAN_POINT('',(0.0165,0.0030542614722702,0.0126361182276936));
#11618=CARTESIAN_POINT('',(0.0165,0.00305426147237052,0.012636118227661));
#11619=CARTESIAN_POINT('',(0.0165,0.00300259945997777,0.0124771189027652));
#11620=CARTESIAN_POINT('',(0.0165,0.00295093744758501,0.0123181195778693));
#11621=CARTESIAN_POINT('',(0.0165,0.00289927543519226,0.0121591202529734));
#11622=CARTESIAN_POINT('',(-0.0005,0.0029767684505,0.012397619231));
#11623=CARTESIAN_POINT('',(0.0165,0.003054261508,0.012636118338));
#11624=CARTESIAN_POINT('',(0.00550000000333333,0.003054261508,0.012636118338));
#11625=CARTESIAN_POINT('',(-0.00549999999333333,0.003054261508,0.012636118338));
#11626=CARTESIAN_POINT('',(-0.01649999999,0.003054261508,0.012636118338));
#11627=CARTESIAN_POINT('',(-0.016499999995,0.00305426150793331,0.0126361183377947));
#11628=CARTESIAN_POINT('',(-0.01649999999,0.003054261508,0.012636118338));
#11629=CARTESIAN_POINT('',(-0.0168333333266667,0.003054261508,0.012636118338));
#11630=CARTESIAN_POINT('',(-0.0171666666633333,0.003054261508,0.012636118338));
#11631=CARTESIAN_POINT('',(-0.0175,0.003054261508,0.012636118338));
#11632=CARTESIAN_POINT('',(-0.0175,0.003054261507645,0.0126361183377328));
#11633=CARTESIAN_POINT('',(-0.0175,0.003054261508,0.012636118338));
#11634=CARTESIAN_POINT('',(-0.0175,0.00300259946966667,0.0124771189333333));
#11635=CARTESIAN_POINT('',(-0.0175,0.00295093743133333,0.0123181195286667));
#11636=CARTESIAN_POINT('',(-0.0175,0.002899275393,0.012159120124));
#11637=CARTESIAN_POINT('',(-0.0175,0.002713045933,0.0148272384279999));
#11638=CARTESIAN_POINT('',(-0.0175,0.00502298787693344,0.0167636390075219));
#11639=CARTESIAN_POINT('',(-0.0175,0.00436674575360062,0.0153877987840808));
#11640=CARTESIAN_POINT('',(-0.0175,0.0037105036302678,0.0140119585606397));
#11641=CARTESIAN_POINT('',(-0.0175,0.00305426150693498,0.0126361183371986));
#11642=CARTESIAN_POINT('',(-0.0174999997505,0.00502298787463437,0.0167636390086185));
#11643=CARTESIAN_POINT('',(-0.0175000000005,0.,0.));
#11644=CARTESIAN_POINT('',(-0.0174999998752501,0.000403104009047257,0.0174953565861415));
#11645=CARTESIAN_POINT('',(-0.0175,0.00100000000007961,0.0129614813976545));
#11646=CARTESIAN_POINT('',(-0.0175,0.000801034669530588,0.0144727731271232));
#11647=CARTESIAN_POINT('',(-0.0175,0.000602069338981565,0.0159840648565919));
#11648=CARTESIAN_POINT('',(-0.0175,0.000403104008432543,0.0174953565860606));
#11649=CARTESIAN_POINT('',(-0.0175,0.00100000000005307,0.0129614813974363));
#11650=CARTESIAN_POINT('',(-0.0175,0.00100000000007961,0.012459935909242));
#11651=CARTESIAN_POINT('',(-0.0175,0.00100000000007961,0.0126271177387128));
#11652=CARTESIAN_POINT('',(-0.0175,0.00100000000007961,0.0127942995681836));
#11653=CARTESIAN_POINT('',(-0.0175,0.00100000000007961,0.0129614813976545));
#11654=CARTESIAN_POINT('',(-0.0005,0.001,0.0127107085955));
#11655=CARTESIAN_POINT('',(-0.0175,0.001,0.012961481397));
#11656=CARTESIAN_POINT('',(-0.0171666666633333,0.001,0.012961481397));
#11657=CARTESIAN_POINT('',(-0.0168333333266667,0.001,0.012961481397));
#11658=CARTESIAN_POINT('',(-0.01649999999,0.001,0.012961481397));
#11659=CARTESIAN_POINT('',(-0.016499999995,0.00100000000001226,0.0129614813969069));
#11660=CARTESIAN_POINT('',(-0.01649999999,0.001,0.012961481397));
#11661=CARTESIAN_POINT('',(-0.00549999999333333,0.001,0.012961481397));
#11662=CARTESIAN_POINT('',(0.00550000000333333,0.001,0.012961481397));
#11663=CARTESIAN_POINT('',(0.0165,0.001,0.012961481397));
#11664=CARTESIAN_POINT('',(0.0165,0.001,0.0129614811469079));
#11665=CARTESIAN_POINT('',(0.0165,0.001,0.0129614811469079));
#11666=CARTESIAN_POINT('',(0.0165,0.001,0.0127942993626052));
#11667=CARTESIAN_POINT('',(0.0165,0.001,0.0126271175783026));
#11668=CARTESIAN_POINT('',(0.0165,0.001,0.012459935794));
#11669=CARTESIAN_POINT('',(0.0165,-1.73472347597681E-19,0.0127315880896833));
#11670=CARTESIAN_POINT('',(0.0165,0.,0.));
#11671=CARTESIAN_POINT('',(0.0165,-0.001,0.0129614812809713));
#11672=CARTESIAN_POINT('',(0.0165,-0.001,0.0129614812809713));
#11673=CARTESIAN_POINT('',(0.0165,-0.001,0.0127942994972893));
#11674=CARTESIAN_POINT('',(0.0165,-0.001,0.0126271177136073));
#11675=CARTESIAN_POINT('',(0.0165,-0.001,0.0124599359299253));
#11676=CARTESIAN_POINT('',(-0.0005,-0.001,0.0127107085955));
#11677=CARTESIAN_POINT('',(0.0165,-0.001,0.012961481397));
#11678=CARTESIAN_POINT('',(0.00550000000333333,-0.001,0.012961481397));
#11679=CARTESIAN_POINT('',(-0.00549999999333333,-0.001,0.012961481397));
#11680=CARTESIAN_POINT('',(-0.01649999999,-0.001,0.012961481397));
#11681=CARTESIAN_POINT('',(-0.016499999995,-0.001,0.0129614813969079));
#11682=CARTESIAN_POINT('',(-0.01649999999,-0.001,0.012961481397));
#11683=CARTESIAN_POINT('',(-0.0168333333266667,-0.001,0.012961481397));
#11684=CARTESIAN_POINT('',(-0.0171666666633333,-0.001,0.012961481397));
#11685=CARTESIAN_POINT('',(-0.0175,-0.001,0.012961481397));
#11686=CARTESIAN_POINT('',(-0.0175,-0.00100000000002654,0.0129614813972181));
#11687=CARTESIAN_POINT('',(-0.0175,-0.001,0.012961481397));
#11688=CARTESIAN_POINT('',(-0.0175,-0.001,0.0127942995293333));
#11689=CARTESIAN_POINT('',(-0.0175,-0.001,0.0126271176616667));
#11690=CARTESIAN_POINT('',(-0.0175,-0.001,0.012459935794));
#11691=CARTESIAN_POINT('',(-0.0175,-0.002713045933,0.0148272384279999));
#11692=CARTESIAN_POINT('',(-0.0175,-0.00040310398916736,0.0174953567323942));
#11693=CARTESIAN_POINT('',(-0.0175,-0.00060206932613811,0.0159840649541476));
#11694=CARTESIAN_POINT('',(-0.0175,-0.00080103466310886,0.014472773175901));
#11695=CARTESIAN_POINT('',(-0.0175,-0.00100000000007961,0.0129614813976545));
#11696=CARTESIAN_POINT('',(-0.0174999997505,-0.00040310398550689,0.0174953567319123));
#11697=CARTESIAN_POINT('',(-0.0175000000005,0.,0.));
#11698=CARTESIAN_POINT('',(-0.0174999998752501,-0.00502298781032175,0.0167636388765541));
#11699=CARTESIAN_POINT('',(-0.0175,-0.00305426150693499,0.0126361183371986));
#11700=CARTESIAN_POINT('',(-0.0175,-0.00371050360918903,0.0140119585164471));
#11701=CARTESIAN_POINT('',(-0.0175,-0.00436674571144307,0.0153877986956956));
#11702=CARTESIAN_POINT('',(-0.0175,-0.00502298781369711,0.0167636388749442));
#11703=CARTESIAN_POINT('',(-0.0175,-0.00305426150728999,0.0126361183374657));
#11704=CARTESIAN_POINT('',(-0.0175,-0.00289927542916025,0.0121591202350179));
#11705=CARTESIAN_POINT('',(-0.0175,-0.00295093745508516,0.0123181196024115));
#11706=CARTESIAN_POINT('',(-0.0175,-0.00300259948101008,0.012477118969805));
#11707=CARTESIAN_POINT('',(-0.0175,-0.00305426150693499,0.0126361183371986));
#11708=CARTESIAN_POINT('',(-0.0005,-0.0029767684505,0.012397619231));
#11709=CARTESIAN_POINT('',(-0.0175,-0.003054261508,0.012636118338));
#11710=CARTESIAN_POINT('',(-0.0171666666633333,-0.003054261508,0.012636118338));
#11711=CARTESIAN_POINT('',(-0.0168333333266667,-0.003054261508,0.012636118338));
#11712=CARTESIAN_POINT('',(-0.01649999999,-0.003054261508,0.012636118338));
#11713=CARTESIAN_POINT('',(-0.016499999995,-0.00305426150790531,0.0126361183378015));
#11714=CARTESIAN_POINT('',(-0.01649999999,-0.003054261508,0.012636118338));
#11715=CARTESIAN_POINT('',(-0.00549999999333333,-0.003054261508,0.012636118338));
#11716=CARTESIAN_POINT('',(0.00550000000333333,-0.003054261508,0.012636118338));
#11717=CARTESIAN_POINT('',(0.0165,-0.003054261508,0.012636118338));
#11718=CARTESIAN_POINT('',(0.0165,-0.00305426143067905,0.0126361181000306));
#11719=CARTESIAN_POINT('',(0.0165,-0.00305426143067905,0.0126361181000306));
#11720=CARTESIAN_POINT('',(0.0165,-0.00300259941811937,0.0124771187746871));
#11721=CARTESIAN_POINT('',(0.0165,-0.00295093740555969,0.0123181194493435));
#11722=CARTESIAN_POINT('',(0.0165,-0.002899275393,0.012159120124));
#11723=CARTESIAN_POINT('',(0.0165,-0.0039278249665,0.0120886022365));
#11724=CARTESIAN_POINT('',(0.0165,0.,0.));
#11725=CARTESIAN_POINT('',(0.0165,-0.00495637450404248,0.0120180842387746));
#11726=CARTESIAN_POINT('',(0.0165,-0.00495637450391302,0.0120180842388167));
#11727=CARTESIAN_POINT('',(0.0165,-0.00490471249152739,0.0118590849139427));
#11728=CARTESIAN_POINT('',(0.0165,-0.00485305047914175,0.0117000855890688));
#11729=CARTESIAN_POINT('',(0.0165,-0.00480138846675611,0.0115410862641948));
#11730=CARTESIAN_POINT('',(-0.0005,-0.004878881483,0.011779585242));
#11731=CARTESIAN_POINT('',(0.0165,-0.00495637454,0.012018084349));
#11732=CARTESIAN_POINT('',(0.00550000000333333,-0.00495637454,0.012018084349));
#11733=CARTESIAN_POINT('',(-0.00549999999333332,-0.00495637454,0.012018084349));
#11734=CARTESIAN_POINT('',(-0.01649999999,-0.00495637454,0.012018084349));
#11735=CARTESIAN_POINT('',(-0.016499999995,-0.00495637453999739,0.0120180843489919));
#11736=CARTESIAN_POINT('',(-0.01649999999,-0.00495637454,0.012018084349));
#11737=CARTESIAN_POINT('',(-0.0168333333266667,-0.00495637454,0.012018084349));
#11738=CARTESIAN_POINT('',(-0.0171666666633333,-0.00495637454,0.012018084349));
#11739=CARTESIAN_POINT('',(-0.0175,-0.00495637454,0.012018084349));
#11740=CARTESIAN_POINT('',(-0.0175,-0.00495637454010061,0.0120180843492958));
#11741=CARTESIAN_POINT('',(-0.0175,-0.00495637454,0.012018084349));
#11742=CARTESIAN_POINT('',(-0.0175,-0.004904712502,0.0118590849443333));
#11743=CARTESIAN_POINT('',(-0.0175,-0.004853050464,0.0117000855396667));
#11744=CARTESIAN_POINT('',(-0.0175,-0.004801388426,0.011541086135));
#11745=CARTESIAN_POINT('',(-0.0175,-0.0073793915595,0.0135912960505));
#11746=CARTESIAN_POINT('',(-0.0175,-0.00578973722584464,0.0165145070408609));
#11747=CARTESIAN_POINT('',(-0.0175,-0.00551194966399704,0.015015699477203));
#11748=CARTESIAN_POINT('',(-0.0175,-0.00523416210214944,0.0135168919135451));
#11749=CARTESIAN_POINT('',(-0.0175,-0.00495637454030183,0.0120180843498873));
#11750=CARTESIAN_POINT('',(-0.0174999997505,-0.00578973723556005,0.0165145070390602));
#11751=CARTESIAN_POINT('',(-0.0175000000005,0.,0.));
#11752=CARTESIAN_POINT('',(-0.0174999998752501,-0.00995739459343785,0.0143909793903514));
#11753=CARTESIAN_POINT('',(-0.0175,-0.00680955061903612,0.0110738439744768));
#11754=CARTESIAN_POINT('',(-0.0175,-0.0078588319435722,0.0121795557800194));
#11755=CARTESIAN_POINT('',(-0.0175,-0.00890811326810827,0.0132852675855619));
#11756=CARTESIAN_POINT('',(-0.0175,-0.00995739459264434,0.0143909793911044));
#11757=CARTESIAN_POINT('',(-0.0175,-0.00680955061902408,0.0110738439746512));
#11758=CARTESIAN_POINT('',(-0.0175,-0.00651474957677916,0.0106680851534263));
#11759=CARTESIAN_POINT('',(-0.0175,-0.00661301659086482,0.0108033380937765));
#11760=CARTESIAN_POINT('',(-0.0175,-0.00671128360495047,0.0109385910341267));
#11761=CARTESIAN_POINT('',(-0.0175,-0.00680955061903612,0.0110738439744768));
#11762=CARTESIAN_POINT('',(-0.0005,-0.00666215006449998,0.010870964517));
#11763=CARTESIAN_POINT('',(-0.0175,-0.00680955061899999,0.011073843975));
#11764=CARTESIAN_POINT('',(-0.0171666666633333,-0.00680955061899999,0.011073843975));
#11765=CARTESIAN_POINT('',(-0.0168333333266667,-0.00680955061899999,0.011073843975));
#11766=CARTESIAN_POINT('',(-0.01649999999,-0.00680955061899999,0.011073843975));
#11767=CARTESIAN_POINT('',(-0.016499999995,-0.00680955061879209,0.0110738439747809));
#11768=CARTESIAN_POINT('',(-0.01649999999,-0.00680955061899999,0.011073843975));
#11769=CARTESIAN_POINT('',(-0.00549999999333334,-0.00680955061899999,0.011073843975));
#11770=CARTESIAN_POINT('',(0.00550000000333334,-0.00680955061899999,0.011073843975));
#11771=CARTESIAN_POINT('',(0.0165,-0.00680955061899999,0.011073843975));
#11772=CARTESIAN_POINT('',(0.0165,-0.00680955047187945,0.011073843772506));
#11773=CARTESIAN_POINT('',(0.0165,-0.00680955047187945,0.011073843772506));
#11774=CARTESIAN_POINT('',(0.0165,-0.0067112834845863,0.010938590868004));
#11775=CARTESIAN_POINT('',(0.0165,-0.00661301649729314,0.010803337963502));
#11776=CARTESIAN_POINT('',(0.0165,-0.00651474950999999,0.010668085059));
#11777=CARTESIAN_POINT('',(0.0165,-0.0074711670585,0.0102831792645));
#11778=CARTESIAN_POINT('',(0.0165,0.,0.));
#11779=CARTESIAN_POINT('',(0.0165,-0.00842758453894735,0.00989827337663452));
#11780=CARTESIAN_POINT('',(0.0165,-0.00842758453880426,0.00989827337673848));
#11781=CARTESIAN_POINT('',(0.0165,-0.00832931755194793,0.00976302047256686));
#11782=CARTESIAN_POINT('',(0.0165,-0.0082310505650916,0.00962776756839523));
#11783=CARTESIAN_POINT('',(0.0165,-0.00813278357823527,0.00949251466422361));
#11784=CARTESIAN_POINT('',(-0.0005,-0.00828018405299999,0.00969539401200001));
#11785=CARTESIAN_POINT('',(0.0165,-0.00842758460699999,0.00989827347000001));
#11786=CARTESIAN_POINT('',(0.00550000000333334,-0.00842758460699999,0.00989827347000001));
#11787=CARTESIAN_POINT('',(-0.00549999999333334,-0.00842758460699999,0.00989827347000001));
#11788=CARTESIAN_POINT('',(-0.01649999999,-0.00842758460699999,0.00989827347000001));
#11789=CARTESIAN_POINT('',(-0.016499999995,-0.00842758460705612,0.00989827347007726));
#11790=CARTESIAN_POINT('',(-0.01649999999,-0.00842758460699999,0.00989827347000001));
#11791=CARTESIAN_POINT('',(-0.0168333333266667,-0.00842758460699999,0.00989827347000001));
#11792=CARTESIAN_POINT('',(-0.0171666666633333,-0.00842758460699999,0.00989827347000001));
#11793=CARTESIAN_POINT('',(-0.0175,-0.00842758460699999,0.00989827347000001));
#11794=CARTESIAN_POINT('',(-0.0175,-0.00842758460672372,0.0098982734697996));
#11795=CARTESIAN_POINT('',(-0.0175,-0.00842758460699999,0.00989827347000001));
#11796=CARTESIAN_POINT('',(-0.0175,-0.00832931757099999,0.00976302049800001));
#11797=CARTESIAN_POINT('',(-0.0175,-0.00823105053499999,0.00962776752600001));
#11798=CARTESIAN_POINT('',(-0.0175,-0.00813278349899999,0.00949251455400001));
#11799=CARTESIAN_POINT('',(-0.0175,-0.011024942919,0.011024942919));
#11800=CARTESIAN_POINT('',(-0.0175,-0.0106096306502694,0.0139171023374371));
#11801=CARTESIAN_POINT('',(-0.0175,-0.0098822819689033,0.0125774927147576));
#11802=CARTESIAN_POINT('',(-0.0175,-0.00915493328753723,0.0112378830920782));
#11803=CARTESIAN_POINT('',(-0.0175,-0.00842758460617116,0.00989827346939878));
#11804=CARTESIAN_POINT('',(-0.0174999997505,-0.0106096306493144,0.0139171023379556));
#11805=CARTESIAN_POINT('',(-0.0175000000005,0.,0.));
#11806=CARTESIAN_POINT('',(-0.0174999998752501,-0.0139171022089875,0.0106096305806968));
#11807=CARTESIAN_POINT('',(-0.0175,-0.00989827346939877,0.00842758460617117));
#11808=CARTESIAN_POINT('',(-0.0175,-0.0112378830492854,0.00915493326430265));
#11809=CARTESIAN_POINT('',(-0.0175,-0.0125774926291721,0.00988228192243413));
#11810=CARTESIAN_POINT('',(-0.0175,-0.0139171022090587,0.0106096305805656));
#11811=CARTESIAN_POINT('',(-0.0175,-0.00989827346959919,0.00842758460644744));
#11812=CARTESIAN_POINT('',(-0.0175,-0.00949251464660495,0.00813278356807117));
#11813=CARTESIAN_POINT('',(-0.0175,-0.00962776758753623,0.00823105058077117));
#11814=CARTESIAN_POINT('',(-0.0175,-0.0097630205284675,0.00832931759347117));
#11815=CARTESIAN_POINT('',(-0.0175,-0.00989827346939877,0.00842758460617117));
#11816=CARTESIAN_POINT('',(-0.0005,-0.009695394012,0.00828018405299999));
#11817=CARTESIAN_POINT('',(-0.0175,-0.00989827347000001,0.00842758460699999));
#11818=CARTESIAN_POINT('',(-0.0171666666633333,-0.00989827347000001,0.00842758460699999));
#11819=CARTESIAN_POINT('',(-0.0168333333266667,-0.00989827347000001,0.00842758460699999));
#11820=CARTESIAN_POINT('',(-0.01649999999,-0.00989827347000001,0.00842758460699999));
#11821=CARTESIAN_POINT('',(-0.016499999995,-0.00989827347008551,0.00842758460704643));
#11822=CARTESIAN_POINT('',(-0.01649999999,-0.00989827347000001,0.00842758460699999));
#11823=CARTESIAN_POINT('',(-0.00549999999333333,-0.00989827347000001,0.00842758460699999));
#11824=CARTESIAN_POINT('',(0.00550000000333333,-0.00989827347000001,0.00842758460699999));
#11825=CARTESIAN_POINT('',(0.0165,-0.00989827347000001,0.00842758460699999));
#11826=CARTESIAN_POINT('',(0.0165,-0.00989827326782301,0.00842758446010981));
#11827=CARTESIAN_POINT('',(0.0165,-0.00989827326782301,0.00842758446010981));
#11828=CARTESIAN_POINT('',(0.0165,-0.00976302036321534,0.0083293174730732));
#11829=CARTESIAN_POINT('',(0.0165,-0.00962776745860767,0.0082310504860366));
#11830=CARTESIAN_POINT('',(0.0165,-0.009492514554,0.00813278349899999));
#11831=CARTESIAN_POINT('',(0.0165,-0.0102831792645,0.0074711670585));
#11832=CARTESIAN_POINT('',(0.0165,0.,0.));
#11833=CARTESIAN_POINT('',(0.0165,-0.0110738438809193,0.0068095505505698));
#11834=CARTESIAN_POINT('',(0.0165,-0.0110738438809557,0.0068095505505197));
#11835=CARTESIAN_POINT('',(0.0165,-0.0109385909767278,0.00671128356362246));
#11836=CARTESIAN_POINT('',(0.0165,-0.0108033380724998,0.00661301657672522));
#11837=CARTESIAN_POINT('',(0.0165,-0.0106680851682719,0.00651474958982798));
#11838=CARTESIAN_POINT('',(-0.0005,-0.010870964517,0.00666215006449997));
#11839=CARTESIAN_POINT('',(0.0165,-0.011073843975,0.00680955061899998));
#11840=CARTESIAN_POINT('',(0.00550000000333333,-0.011073843975,0.00680955061899998));
#11841=CARTESIAN_POINT('',(-0.00549999999333332,-0.011073843975,0.00680955061899998));
#11842=CARTESIAN_POINT('',(-0.01649999999,-0.011073843975,0.00680955061899998));
#11843=CARTESIAN_POINT('',(-0.016499999995,-0.0110738439747602,0.00680955061882576));
#11844=CARTESIAN_POINT('',(-0.01649999999,-0.011073843975,0.00680955061899998));
#11845=CARTESIAN_POINT('',(-0.0168333333266667,-0.011073843975,0.00680955061899998));
#11846=CARTESIAN_POINT('',(-0.0171666666633333,-0.011073843975,0.00680955061899998));
#11847=CARTESIAN_POINT('',(-0.0175,-0.011073843975,0.00680955061899998));
#11848=CARTESIAN_POINT('',(-0.0175,-0.0110738439748256,0.00680955061901203));
#11849=CARTESIAN_POINT('',(-0.0175,-0.011073843975,0.00680955061899998));
#11850=CARTESIAN_POINT('',(-0.0175,-0.010938591003,0.00671128358266665));
#11851=CARTESIAN_POINT('',(-0.0175,-0.010803338031,0.00661301654633331));
#11852=CARTESIAN_POINT('',(-0.0175,-0.010668085059,0.00651474950999998));
#11853=CARTESIAN_POINT('',(-0.0175,-0.0135912960505,0.0073793915595));
#11854=CARTESIAN_POINT('',(-0.0175,-0.0143909794982839,0.00995739469435391));
#11855=CARTESIAN_POINT('',(-0.0175,-0.0132852676570149,0.00890811333591465));
#11856=CARTESIAN_POINT('',(-0.0175,-0.0121795558157459,0.00785883197747539));
#11857=CARTESIAN_POINT('',(-0.0175,-0.0110738439744768,0.00680955061903613));
#11858=CARTESIAN_POINT('',(-0.0174999997505,-0.0143909794958243,0.00995739469694575));
#11859=CARTESIAN_POINT('',(-0.0175000000005,0.,0.));
#11860=CARTESIAN_POINT('',(-0.0174999998752501,-0.0165145068989394,0.00578973719647625));
#11861=CARTESIAN_POINT('',(-0.0175,-0.0120180843498873,0.00495637454030183));
#11862=CARTESIAN_POINT('',(-0.0175,-0.013516891866055,0.00523416209334765));
#11863=CARTESIAN_POINT('',(-0.0175,-0.0150156993822226,0.00551194964639347));
#11864=CARTESIAN_POINT('',(-0.0175,-0.0165145068983903,0.00578973719943929));
#11865=CARTESIAN_POINT('',(-0.0175,-0.0120180843495915,0.00495637454020122));
#11866=CARTESIAN_POINT('',(-0.0175,-0.0115410862465846,0.00480138846215994));
#11867=CARTESIAN_POINT('',(-0.0175,-0.0117000856143522,0.00485305048820723));
#11868=CARTESIAN_POINT('',(-0.0175,-0.0118590849821197,0.00490471251425453));
#11869=CARTESIAN_POINT('',(-0.0175,-0.0120180843498873,0.00495637454030183));
#11870=CARTESIAN_POINT('',(-0.0005,-0.011779585242,0.004878881483));
#11871=CARTESIAN_POINT('',(-0.0175,-0.012018084349,0.00495637454));
#11872=CARTESIAN_POINT('',(-0.0171666666633333,-0.012018084349,0.00495637454));
#11873=CARTESIAN_POINT('',(-0.0168333333266667,-0.012018084349,0.00495637454));
#11874=CARTESIAN_POINT('',(-0.01649999999,-0.012018084349,0.00495637454));
#11875=CARTESIAN_POINT('',(-0.016499999995,-0.0120180843489915,0.00495637453999843));
#11876=CARTESIAN_POINT('',(-0.01649999999,-0.012018084349,0.00495637454));
#11877=CARTESIAN_POINT('',(-0.00549999999333334,-0.012018084349,0.00495637454));
#11878=CARTESIAN_POINT('',(0.00550000000333334,-0.012018084349,0.00495637454));
#11879=CARTESIAN_POINT('',(0.0165,-0.012018084349,0.00495637454));
#11880=CARTESIAN_POINT('',(0.0165,-0.0120180841112278,0.00495637446274314));
#11881=CARTESIAN_POINT('',(0.0165,-0.0120180841112278,0.00495637446274314));
#11882=CARTESIAN_POINT('',(0.0165,-0.0118590847858185,0.00490471245049542));
#11883=CARTESIAN_POINT('',(0.0165,-0.0117000854604093,0.00485305043824771));
#11884=CARTESIAN_POINT('',(0.0165,-0.011541086135,0.004801388426));
#11885=CARTESIAN_POINT('',(0.0165,-0.0120886022365,0.00392782496649999));
#11886=CARTESIAN_POINT('',(0.0165,0.,0.));
#11887=CARTESIAN_POINT('',(0.0165,-0.0126361182276936,0.0030542614722702));
#11888=CARTESIAN_POINT('',(0.0165,-0.012636118227661,0.00305426147237052));
#11889=CARTESIAN_POINT('',(0.0165,-0.0124771189027327,0.0030025994599672));
#11890=CARTESIAN_POINT('',(0.0165,-0.0123181195778043,0.00295093744756389));
#11891=CARTESIAN_POINT('',(0.0165,-0.0121591202528759,0.00289927543516057));
#11892=CARTESIAN_POINT('',(-0.0005,-0.012397619231,0.0029767684505));
#11893=CARTESIAN_POINT('',(0.0165,-0.012636118338,0.003054261508));
#11894=CARTESIAN_POINT('',(0.00550000000333333,-0.012636118338,0.003054261508));
#11895=CARTESIAN_POINT('',(-0.00549999999333333,-0.012636118338,0.003054261508));
#11896=CARTESIAN_POINT('',(-0.01649999999,-0.012636118338,0.003054261508));
#11897=CARTESIAN_POINT('',(-0.016499999995,-0.0126361183377947,0.00305426150793331));
#11898=CARTESIAN_POINT('',(-0.01649999999,-0.012636118338,0.003054261508));
#11899=CARTESIAN_POINT('',(-0.0168333333266667,-0.012636118338,0.003054261508));
#11900=CARTESIAN_POINT('',(-0.0171666666633333,-0.012636118338,0.003054261508));
#11901=CARTESIAN_POINT('',(-0.0175,-0.012636118338,0.003054261508));
#11902=CARTESIAN_POINT('',(-0.0175,-0.0126361183377328,0.003054261507645));
#11903=CARTESIAN_POINT('',(-0.0175,-0.012636118338,0.003054261508));
#11904=CARTESIAN_POINT('',(-0.0175,-0.0124771189333333,0.00300259946966667));
#11905=CARTESIAN_POINT('',(-0.0175,-0.0123181195286667,0.00295093743133333));
#11906=CARTESIAN_POINT('',(-0.0175,-0.012159120124,0.002899275393));
#11907=CARTESIAN_POINT('',(-0.0175,-0.014827238428,0.002713045933));
#11908=CARTESIAN_POINT('',(-0.0175,-0.0167636390070252,0.00502298787669651));
#11909=CARTESIAN_POINT('',(-0.0175,-0.0153877987837496,0.00436674575344267));
#11910=CARTESIAN_POINT('',(-0.0175,-0.0140119585604741,0.00371050363018883));
#11911=CARTESIAN_POINT('',(-0.0175,-0.0126361183371986,0.00305426150693499));
#11912=CARTESIAN_POINT('',(-0.0174999997505,-0.0167636390096488,0.00502298787119609));
#11913=CARTESIAN_POINT('',(-0.0175000000005,0.,0.));
#11914=CARTESIAN_POINT('',(-0.0174999998752501,-0.0174953565861828,0.000403104007253075));
#11915=CARTESIAN_POINT('',(-0.0175,-0.0129614813976545,0.00100000000007961));
#11916=CARTESIAN_POINT('',(-0.0175,-0.0144727731272141,0.000801034669518615));
#11917=CARTESIAN_POINT('',(-0.0175,-0.0159840648567738,0.000602069338957621));
#11918=CARTESIAN_POINT('',(-0.0175,-0.0174953565863334,0.000403104008396626));
#11919=CARTESIAN_POINT('',(-0.0175,-0.0129614813974363,0.00100000000005307));
#11920=CARTESIAN_POINT('',(-0.0175,-0.0124599359093445,0.00100000000007961));
#11921=CARTESIAN_POINT('',(-0.0175,-0.0126271177387812,0.00100000000007961));
#11922=CARTESIAN_POINT('',(-0.0175,-0.0127942995682178,0.00100000000007961));
#11923=CARTESIAN_POINT('',(-0.0175,-0.0129614813976545,0.00100000000007961));
#11924=CARTESIAN_POINT('',(-0.0005,-0.0127107085955,0.001));
#11925=CARTESIAN_POINT('',(-0.0175,-0.012961481397,0.001));
#11926=CARTESIAN_POINT('',(-0.0171666666633333,-0.012961481397,0.001));
#11927=CARTESIAN_POINT('',(-0.0168333333266667,-0.012961481397,0.001));
#11928=CARTESIAN_POINT('',(-0.01649999999,-0.012961481397,0.001));
#11929=CARTESIAN_POINT('',(-0.016499999995,-0.0129614813969069,0.00100000000001226));
#11930=CARTESIAN_POINT('',(-0.01649999999,-0.012961481397,0.001));
#11931=CARTESIAN_POINT('',(-0.00549999999333333,-0.012961481397,0.001));
#11932=CARTESIAN_POINT('',(0.00550000000333333,-0.012961481397,0.001));
#11933=CARTESIAN_POINT('',(0.0165,-0.012961481397,0.001));
#11934=CARTESIAN_POINT('',(0.0165,-0.0129614811469079,0.001));
#11935=CARTESIAN_POINT('',(0.0165,-0.0129614811469079,0.001));
#11936=CARTESIAN_POINT('',(0.0165,-0.0127942993626052,0.001));
#11937=CARTESIAN_POINT('',(0.0165,-0.0126271175783026,0.001));
#11938=CARTESIAN_POINT('',(0.0165,-0.012459935794,0.001));
#11939=CARTESIAN_POINT('',(0.0165,-0.0127315880896833,-1.56125112837913E-19));
#11940=CARTESIAN_POINT('',(0.0165,0.,0.));
#11941=CARTESIAN_POINT('',(0.0165,-0.0129614812809713,-0.001));
#11942=CARTESIAN_POINT('',(0.0165,-0.0129614812809713,-0.001));
#11943=CARTESIAN_POINT('',(0.0165,-0.0127942994972252,-0.001));
#11944=CARTESIAN_POINT('',(0.0165,-0.0126271177134791,-0.001));
#11945=CARTESIAN_POINT('',(0.0165,-0.012459935929733,-0.001));
#11946=CARTESIAN_POINT('',(-0.0005,-0.0127107085955,-0.001));
#11947=CARTESIAN_POINT('',(0.0165,-0.012961481397,-0.001));
#11948=CARTESIAN_POINT('',(0.00550000000333333,-0.012961481397,-0.001));
#11949=CARTESIAN_POINT('',(-0.00549999999333333,-0.012961481397,-0.001));
#11950=CARTESIAN_POINT('',(-0.01649999999,-0.012961481397,-0.001));
#11951=CARTESIAN_POINT('',(-0.016499999995,-0.0129614813969079,-0.001));
#11952=CARTESIAN_POINT('',(-0.01649999999,-0.012961481397,-0.001));
#11953=CARTESIAN_POINT('',(-0.0168333333266667,-0.012961481397,-0.001));
#11954=CARTESIAN_POINT('',(-0.0171666666633333,-0.012961481397,-0.001));
#11955=CARTESIAN_POINT('',(-0.0175,-0.012961481397,-0.001));
#11956=CARTESIAN_POINT('',(-0.0175,-0.0129614813972181,-0.00100000000002654));
#11957=CARTESIAN_POINT('',(-0.0175,-0.012961481397,-0.001));
#11958=CARTESIAN_POINT('',(-0.0175,-0.0127942995293333,-0.001));
#11959=CARTESIAN_POINT('',(-0.0175,-0.0126271176616667,-0.001));
#11960=CARTESIAN_POINT('',(-0.0175,-0.012459935794,-0.001));
#11961=CARTESIAN_POINT('',(-0.0175,-0.014827238428,-0.002713045933));
#11962=CARTESIAN_POINT('',(-0.0175,-0.0174953567315252,-0.000403103989281762));
#11963=CARTESIAN_POINT('',(-0.0175,-0.0159840649535683,-0.000602069326214379));
#11964=CARTESIAN_POINT('',(-0.0175,-0.0144727731756114,-0.000801034663146997));
#11965=CARTESIAN_POINT('',(-0.0175,-0.0129614813976545,-0.00100000000007961));
#11966=CARTESIAN_POINT('',(-0.0174999998755,-0.0174953567317806,-0.000403103991221634));
#11967=CARTESIAN_POINT('',(-0.0175000000005,0.,0.));
#11968=CARTESIAN_POINT('',(-0.0174999998752501,-0.016763638875588,-0.00502298781354615));
#11969=CARTESIAN_POINT('',(-0.0175,-0.0126361183371986,-0.00305426150693499));
#11970=CARTESIAN_POINT('',(-0.0175,-0.0140119585166024,-0.00371050360926309));
#11971=CARTESIAN_POINT('',(-0.0175,-0.0153877986960062,-0.00436674571159119));
#11972=CARTESIAN_POINT('',(-0.0175,-0.01676363887541,-0.0050229878139193));
#11973=CARTESIAN_POINT('',(-0.0175,-0.0126361183374657,-0.00305426150728999));
#11974=CARTESIAN_POINT('',(-0.0175,-0.0121591202347253,-0.00289927542906519));
#11975=CARTESIAN_POINT('',(-0.0175,-0.0123181196022164,-0.00295093745502179));
#11976=CARTESIAN_POINT('',(-0.0175,-0.0124771189697075,-0.00300259948097839));
#11977=CARTESIAN_POINT('',(-0.0175,-0.0126361183371986,-0.00305426150693499));
#11978=CARTESIAN_POINT('',(-0.0005,-0.012397619231,-0.0029767684505));
#11979=CARTESIAN_POINT('',(-0.0175,-0.012636118338,-0.003054261508));
#11980=CARTESIAN_POINT('',(-0.0171666666633333,-0.012636118338,-0.003054261508));
#11981=CARTESIAN_POINT('',(-0.0168333333266667,-0.012636118338,-0.003054261508));
#11982=CARTESIAN_POINT('',(-0.01649999999,-0.012636118338,-0.003054261508));
#11983=CARTESIAN_POINT('',(-0.016499999995,-0.0126361183378015,-0.00305426150790531));
#11984=CARTESIAN_POINT('',(-0.01649999999,-0.012636118338,-0.003054261508));
#11985=CARTESIAN_POINT('',(-0.00549999999333333,-0.012636118338,-0.003054261508));
#11986=CARTESIAN_POINT('',(0.00550000000333333,-0.012636118338,-0.003054261508));
#11987=CARTESIAN_POINT('',(0.0165,-0.012636118338,-0.003054261508));
#11988=CARTESIAN_POINT('',(0.0165,-0.0126361181000306,-0.00305426143067905));
#11989=CARTESIAN_POINT('',(0.0165,-0.0126361181000306,-0.00305426143067905));
#11990=CARTESIAN_POINT('',(0.0165,-0.0124771187746871,-0.00300259941811937));
#11991=CARTESIAN_POINT('',(0.0165,-0.0123181194493435,-0.00295093740555969));
#11992=CARTESIAN_POINT('',(0.0165,-0.012159120124,-0.002899275393));
#11993=CARTESIAN_POINT('',(0.0165,-0.0120886022365,-0.00392782496650001));
#11994=CARTESIAN_POINT('',(0.0165,0.,0.));
#11995=CARTESIAN_POINT('',(0.0165,-0.0120180842387746,-0.00495637450404248));
#11996=CARTESIAN_POINT('',(0.0165,-0.0120180842388167,-0.00495637450391302));
#11997=CARTESIAN_POINT('',(0.0165,-0.0118590849140403,-0.00490471249155908));
#11998=CARTESIAN_POINT('',(0.0165,-0.0117000855892638,-0.00485305047920513));
#11999=CARTESIAN_POINT('',(0.0165,-0.0115410862644874,-0.00480138846685119));
#12000=CARTESIAN_POINT('',(-0.0005,-0.011779585242,-0.004878881483));
#12001=CARTESIAN_POINT('',(0.0165,-0.012018084349,-0.00495637454));
#12002=CARTESIAN_POINT('',(0.00550000000333333,-0.012018084349,-0.00495637454));
#12003=CARTESIAN_POINT('',(-0.00549999999333332,-0.012018084349,-0.00495637454));
#12004=CARTESIAN_POINT('',(-0.01649999999,-0.012018084349,-0.00495637454));
#12005=CARTESIAN_POINT('',(-0.016499999995,-0.0120180843489919,-0.00495637453999739));
#12006=CARTESIAN_POINT('',(-0.01649999999,-0.012018084349,-0.00495637454));
#12007=CARTESIAN_POINT('',(-0.0168333333266667,-0.012018084349,-0.00495637454));
#12008=CARTESIAN_POINT('',(-0.0171666666633333,-0.012018084349,-0.00495637454));
#12009=CARTESIAN_POINT('',(-0.0175,-0.012018084349,-0.00495637454));
#12010=CARTESIAN_POINT('',(-0.0175,-0.0120180843492958,-0.00495637454010061));
#12011=CARTESIAN_POINT('',(-0.0175,-0.012018084349,-0.00495637454));
#12012=CARTESIAN_POINT('',(-0.0175,-0.0118590849443333,-0.004904712502));
#12013=CARTESIAN_POINT('',(-0.0175,-0.0117000855396667,-0.004853050464));
#12014=CARTESIAN_POINT('',(-0.0175,-0.011541086135,-0.004801388426));
#12015=CARTESIAN_POINT('',(-0.0175,-0.0135912960505,-0.0073793915595));
#12016=CARTESIAN_POINT('',(-0.0175,-0.0165145070424843,-0.00578973722614552));
#12017=CARTESIAN_POINT('',(-0.0175,-0.0150156994782853,-0.00551194966419762));
#12018=CARTESIAN_POINT('',(-0.0175,-0.0135168919140863,-0.00523416210224972));
#12019=CARTESIAN_POINT('',(-0.0175,-0.0120180843498873,-0.00495637454030183));
#12020=CARTESIAN_POINT('',(-0.0174999997505,-0.0165145070426227,-0.0057897372253985));
#12021=CARTESIAN_POINT('',(-0.0175000000005,0.,0.));
#12022=CARTESIAN_POINT('',(-0.0174999998752501,-0.0143909793934148,-0.0099573945890104));
#12023=CARTESIAN_POINT('',(-0.0175,-0.0110738439744768,-0.00680955061903612));
#12024=CARTESIAN_POINT('',(-0.0175,-0.0121795557798198,-0.00785883194338278));
#12025=CARTESIAN_POINT('',(-0.0175,-0.0132852675851627,-0.00890811326772944));
#12026=CARTESIAN_POINT('',(-0.0175,-0.0143909793905056,-0.00995739459207609));
#12027=CARTESIAN_POINT('',(-0.0175,-0.0110738439746512,-0.00680955061902408));
#12028=CARTESIAN_POINT('',(-0.0175,-0.0106680851535819,-0.00651474957689222));
#12029=CARTESIAN_POINT('',(-0.0175,-0.0108033380938802,-0.00661301659094019));
#12030=CARTESIAN_POINT('',(-0.0175,-0.0109385910341785,-0.00671128360498816));
#12031=CARTESIAN_POINT('',(-0.0175,-0.0110738439744768,-0.00680955061903612));
#12032=CARTESIAN_POINT('',(-0.0005,-0.010870964517,-0.00666215006449998));
#12033=CARTESIAN_POINT('',(-0.0175,-0.011073843975,-0.00680955061899999));
#12034=CARTESIAN_POINT('',(-0.0171666666633333,-0.011073843975,-0.00680955061899999));
#12035=CARTESIAN_POINT('',(-0.0168333333266667,-0.011073843975,-0.00680955061899999));
#12036=CARTESIAN_POINT('',(-0.01649999999,-0.011073843975,-0.00680955061899999));
#12037=CARTESIAN_POINT('',(-0.016499999995,-0.0110738439747809,-0.00680955061879209));
#12038=CARTESIAN_POINT('',(-0.01649999999,-0.011073843975,-0.00680955061899999));
#12039=CARTESIAN_POINT('',(-0.00549999999333334,-0.011073843975,-0.00680955061899999));
#12040=CARTESIAN_POINT('',(0.00550000000333334,-0.011073843975,-0.00680955061899999));
#12041=CARTESIAN_POINT('',(0.0165,-0.011073843975,-0.00680955061899999));
#12042=CARTESIAN_POINT('',(0.0165,-0.011073843772506,-0.00680955047187945));
#12043=CARTESIAN_POINT('',(0.0165,-0.011073843772506,-0.00680955047187945));
#12044=CARTESIAN_POINT('',(0.0165,-0.010938590868004,-0.0067112834845863));
#12045=CARTESIAN_POINT('',(0.0165,-0.010803337963502,-0.00661301649729314));
#12046=CARTESIAN_POINT('',(0.0165,-0.010668085059,-0.00651474950999999));
#12047=CARTESIAN_POINT('',(0.0165,-0.0102831792645,-0.0074711670585));
#12048=CARTESIAN_POINT('',(0.0165,0.,0.));
#12049=CARTESIAN_POINT('',(0.0165,-0.00989827337663452,-0.00842758453894735));
#12050=CARTESIAN_POINT('',(0.0165,-0.00989827337673848,-0.00842758453880425));
#12051=CARTESIAN_POINT('',(0.0165,-0.00976302047251499,-0.00832931755191023));
#12052=CARTESIAN_POINT('',(0.0165,-0.00962776756829149,-0.00823105056501622));
#12053=CARTESIAN_POINT('',(0.0165,-0.00949251466406799,-0.0081327835781222));
#12054=CARTESIAN_POINT('',(-0.0005,-0.00969539401200001,-0.00828018405299999));
#12055=CARTESIAN_POINT('',(0.0165,-0.00989827347000001,-0.00842758460699999));
#12056=CARTESIAN_POINT('',(0.00550000000333334,-0.00989827347000001,-0.00842758460699999));
#12057=CARTESIAN_POINT('',(-0.00549999999333334,-0.00989827347000001,-0.00842758460699999));
#12058=CARTESIAN_POINT('',(-0.01649999999,-0.00989827347000001,-0.00842758460699999));
#12059=CARTESIAN_POINT('',(-0.016499999995,-0.00989827347007726,-0.00842758460705612));
#12060=CARTESIAN_POINT('',(-0.01649999999,-0.00989827347000001,-0.00842758460699999));
#12061=CARTESIAN_POINT('',(-0.0168333333266667,-0.00989827347000001,-0.00842758460699999));
#12062=CARTESIAN_POINT('',(-0.0171666666633333,-0.00989827347000001,-0.00842758460699999));
#12063=CARTESIAN_POINT('',(-0.0175,-0.00989827347000001,-0.00842758460699999));
#12064=CARTESIAN_POINT('',(-0.0175,-0.0098982734697996,-0.00842758460672372));
#12065=CARTESIAN_POINT('',(-0.0175,-0.00989827347000001,-0.00842758460699999));
#12066=CARTESIAN_POINT('',(-0.0175,-0.00976302049800001,-0.00832931757099999));
#12067=CARTESIAN_POINT('',(-0.0175,-0.00962776752600001,-0.00823105053499999));
#12068=CARTESIAN_POINT('',(-0.0175,-0.00949251455400001,-0.00813278349899999));
#12069=CARTESIAN_POINT('',(-0.0175,-0.011024942919,-0.011024942919));
#12070=CARTESIAN_POINT('',(-0.0175,-0.0139171023365299,-0.0106096306497768));
#12071=CARTESIAN_POINT('',(-0.0175,-0.0125774927141529,-0.00988228196857495));
#12072=CARTESIAN_POINT('',(-0.0175,-0.0112378830917758,-0.00915493328737306));
#12073=CARTESIAN_POINT('',(-0.0175,-0.00989827346939877,-0.00842758460617117));
#12074=CARTESIAN_POINT('',(-0.0174999997505,-0.0139171023338741,-0.0106096306546682));
#12075=CARTESIAN_POINT('',(-0.0175000000005,0.,0.));
#12076=CARTESIAN_POINT('',(-0.0174999998752501,-0.0106096305780199,-0.0139171022110282));
#12077=CARTESIAN_POINT('',(-0.0175,-0.00842758460617116,-0.00989827346939879));
#12078=CARTESIAN_POINT('',(-0.0175,-0.00915493326438473,-0.0112378830494366));
#12079=CARTESIAN_POINT('',(-0.0175,-0.0098822819225983,-0.0125774926294745));
#12080=CARTESIAN_POINT('',(-0.0175,-0.0106096305808119,-0.0139171022095123));
#12081=CARTESIAN_POINT('',(-0.0175,-0.00842758460644744,-0.00989827346959919));
#12082=CARTESIAN_POINT('',(-0.0175,-0.00813278356818423,-0.00949251464676057));
#12083=CARTESIAN_POINT('',(-0.0175,-0.00823105058084654,-0.00962776758763998));
#12084=CARTESIAN_POINT('',(-0.0175,-0.00832931759350885,-0.00976302052851938));
#12085=CARTESIAN_POINT('',(-0.0175,-0.00842758460617116,-0.00989827346939879));
#12086=CARTESIAN_POINT('',(-0.0005,-0.00828018405299999,-0.009695394012));
#12087=CARTESIAN_POINT('',(-0.0175,-0.00842758460699999,-0.00989827347000001));
#12088=CARTESIAN_POINT('',(-0.0171666666633333,-0.00842758460699999,-0.00989827347000001));
#12089=CARTESIAN_POINT('',(-0.0168333333266667,-0.00842758460699999,-0.00989827347000001));
#12090=CARTESIAN_POINT('',(-0.01649999999,-0.00842758460699999,-0.00989827347000001));
#12091=CARTESIAN_POINT('',(-0.016499999995,-0.00842758460704643,-0.00989827347008551));
#12092=CARTESIAN_POINT('',(-0.01649999999,-0.00842758460699999,-0.00989827347000001));
#12093=CARTESIAN_POINT('',(-0.00549999999333333,-0.00842758460699999,-0.00989827347000001));
#12094=CARTESIAN_POINT('',(0.00550000000333333,-0.00842758460699999,-0.00989827347000001));
#12095=CARTESIAN_POINT('',(0.0165,-0.00842758460699999,-0.00989827347000001));
#12096=CARTESIAN_POINT('',(0.0165,-0.00842758446010981,-0.00989827326782301));
#12097=CARTESIAN_POINT('',(0.0165,-0.00842758446010981,-0.00989827326782301));
#12098=CARTESIAN_POINT('',(0.0165,-0.0083293174730732,-0.00976302036321534));
#12099=CARTESIAN_POINT('',(0.0165,-0.0082310504860366,-0.00962776745860767));
#12100=CARTESIAN_POINT('',(0.0165,-0.00813278349899999,-0.009492514554));
#12101=CARTESIAN_POINT('',(0.0165,-0.0074711670585,-0.0102831792645));
#12102=CARTESIAN_POINT('',(0.0165,0.,0.));
#12103=CARTESIAN_POINT('',(0.0165,-0.0068095505505698,-0.0110738438809193));
#12104=CARTESIAN_POINT('',(0.0165,-0.00680955055051969,-0.0110738438809557));
#12105=CARTESIAN_POINT('',(0.0165,-0.00671128356358477,-0.0109385909766759));
#12106=CARTESIAN_POINT('',(0.0165,-0.00661301657664984,-0.0108033380723961));
#12107=CARTESIAN_POINT('',(0.0165,-0.00651474958971492,-0.0106680851681163));
#12108=CARTESIAN_POINT('',(-0.0005,-0.00666215006449997,-0.010870964517));
#12109=CARTESIAN_POINT('',(0.0165,-0.00680955061899998,-0.011073843975));
#12110=CARTESIAN_POINT('',(0.00550000000333333,-0.00680955061899998,-0.011073843975));
#12111=CARTESIAN_POINT('',(-0.00549999999333332,-0.00680955061899998,-0.011073843975));
#12112=CARTESIAN_POINT('',(-0.01649999999,-0.00680955061899998,-0.011073843975));
#12113=CARTESIAN_POINT('',(-0.016499999995,-0.00680955061882576,-0.0110738439747602));
#12114=CARTESIAN_POINT('',(-0.01649999999,-0.00680955061899998,-0.011073843975));
#12115=CARTESIAN_POINT('',(-0.0168333333266667,-0.00680955061899998,-0.011073843975));
#12116=CARTESIAN_POINT('',(-0.0171666666633333,-0.00680955061899998,-0.011073843975));
#12117=CARTESIAN_POINT('',(-0.0175,-0.00680955061899998,-0.011073843975));
#12118=CARTESIAN_POINT('',(-0.0175,-0.00680955061901203,-0.0110738439748256));
#12119=CARTESIAN_POINT('',(-0.0175,-0.00680955061899998,-0.011073843975));
#12120=CARTESIAN_POINT('',(-0.0175,-0.00671128358266665,-0.010938591003));
#12121=CARTESIAN_POINT('',(-0.0175,-0.00661301654633331,-0.010803338031));
#12122=CARTESIAN_POINT('',(-0.0175,-0.00651474950999998,-0.010668085059));
#12123=CARTESIAN_POINT('',(-0.0175,-0.0073793915595,-0.0135912960505));
#12124=CARTESIAN_POINT('',(-0.0175,-0.00995739469364337,-0.0143909794975352));
#12125=CARTESIAN_POINT('',(-0.0175,-0.00890811333544096,-0.0132852676565157));
#12126=CARTESIAN_POINT('',(-0.0175,-0.00785883197723854,-0.0121795558154963));
#12127=CARTESIAN_POINT('',(-0.0175,-0.00680955061903612,-0.0110738439744768));
#12128=CARTESIAN_POINT('',(-0.0174999997505,-0.00995739469140969,-0.0143909794996549));
#12129=CARTESIAN_POINT('',(-0.0175000000005,0.,0.));
#12130=CARTESIAN_POINT('',(-0.0174999998752501,-0.00578973720155703,-0.0165145068971582));
#12131=CARTESIAN_POINT('',(-0.0175,-0.00495637454030183,-0.0120180843498873));
#12132=CARTESIAN_POINT('',(-0.0175,-0.0052341620932975,-0.0135168918657844));
#12133=CARTESIAN_POINT('',(-0.0175,-0.00551194964629317,-0.0150156993816815));
#12134=CARTESIAN_POINT('',(-0.0175,-0.00578973719928885,-0.0165145068975786));
#12135=CARTESIAN_POINT('',(-0.0175,-0.00495637454020122,-0.0120180843495915));
#12136=CARTESIAN_POINT('',(-0.0175,-0.00480138846206486,-0.011541086246292));
#12137=CARTESIAN_POINT('',(-0.0175,-0.00485305048814385,-0.0117000856141571));
#12138=CARTESIAN_POINT('',(-0.0175,-0.00490471251422284,-0.0118590849820222));
#12139=CARTESIAN_POINT('',(-0.0175,-0.00495637454030183,-0.0120180843498873));
#12140=CARTESIAN_POINT('',(-0.0005,-0.004878881483,-0.011779585242));
#12141=CARTESIAN_POINT('',(-0.0175,-0.00495637454,-0.012018084349));
#12142=CARTESIAN_POINT('',(-0.0171666666633333,-0.00495637454,-0.012018084349));
#12143=CARTESIAN_POINT('',(-0.0168333333266667,-0.00495637454,-0.012018084349));
#12144=CARTESIAN_POINT('',(-0.01649999999,-0.00495637454,-0.012018084349));
#12145=CARTESIAN_POINT('',(-0.016499999995,-0.00495637453999843,-0.0120180843489915));
#12146=CARTESIAN_POINT('',(-0.01649999999,-0.00495637454,-0.012018084349));
#12147=CARTESIAN_POINT('',(-0.00549999999333334,-0.00495637454,-0.012018084349));
#12148=CARTESIAN_POINT('',(0.00550000000333334,-0.00495637454,-0.012018084349));
#12149=CARTESIAN_POINT('',(0.0165,-0.00495637454,-0.012018084349));
#12150=CARTESIAN_POINT('',(0.0165,-0.00495637446274314,-0.0120180841112278));
#12151=CARTESIAN_POINT('',(0.0165,-0.00495637446274314,-0.0120180841112278));
#12152=CARTESIAN_POINT('',(0.0165,-0.00490471245049542,-0.0118590847858185));
#12153=CARTESIAN_POINT('',(0.0165,-0.00485305043824771,-0.0117000854604093));
#12154=CARTESIAN_POINT('',(0.0165,-0.004801388426,-0.011541086135));
#12155=CARTESIAN_POINT('',(0.0165,-0.0039278249665,-0.0120886022365));
#12156=CARTESIAN_POINT('',(0.0165,0.,0.));
#12157=CARTESIAN_POINT('',(0.0165,-0.0030542614722702,-0.0126361182276936));
#12158=CARTESIAN_POINT('',(0.0165,-0.00305426147237052,-0.012636118227661));
#12159=CARTESIAN_POINT('',(0.0165,-0.0030025994599989,-0.0124771189028302));
#12160=CARTESIAN_POINT('',(0.0165,-0.00295093744762727,-0.0123181195779993));
#12161=CARTESIAN_POINT('',(0.0165,-0.00289927543525564,-0.0121591202531685));
#12162=CARTESIAN_POINT('',(-0.0005,-0.0029767684505,-0.012397619231));
#12163=CARTESIAN_POINT('',(0.0165,-0.003054261508,-0.012636118338));
#12164=CARTESIAN_POINT('',(0.00550000000333333,-0.003054261508,-0.012636118338));
#12165=CARTESIAN_POINT('',(-0.00549999999333333,-0.003054261508,-0.012636118338));
#12166=CARTESIAN_POINT('',(-0.01649999999,-0.003054261508,-0.012636118338));
#12167=CARTESIAN_POINT('',(-0.016499999995,-0.00305426150793331,-0.0126361183377947));
#12168=CARTESIAN_POINT('',(-0.01649999999,-0.003054261508,-0.012636118338));
#12169=CARTESIAN_POINT('',(-0.0168333333266667,-0.003054261508,-0.012636118338));
#12170=CARTESIAN_POINT('',(-0.0171666666633333,-0.003054261508,-0.012636118338));
#12171=CARTESIAN_POINT('',(-0.0175,-0.003054261508,-0.012636118338));
#12172=CARTESIAN_POINT('',(-0.0175,-0.003054261507645,-0.0126361183377328));
#12173=CARTESIAN_POINT('',(-0.0175,-0.003054261508,-0.012636118338));
#12174=CARTESIAN_POINT('',(-0.0175,-0.00300259946966667,-0.0124771189333333));
#12175=CARTESIAN_POINT('',(-0.0175,-0.00295093743133333,-0.0123181195286667));
#12176=CARTESIAN_POINT('',(-0.0175,-0.002899275393,-0.012159120124));
#12177=CARTESIAN_POINT('',(-0.0175,-0.002713045933,-0.0148272384280001));
#12178=CARTESIAN_POINT('',(-0.0175,-0.0050229878774073,-0.0167636390085154));
#12179=CARTESIAN_POINT('',(-0.0175,-0.00436674575391653,-0.0153877987847431));
#12180=CARTESIAN_POINT('',(-0.0175,-0.00371050363042576,-0.0140119585609708));
#12181=CARTESIAN_POINT('',(-0.0175,-0.00305426150693499,-0.0126361183371985));
#12182=CARTESIAN_POINT('',(-0.0174999997505,-0.00502298788151093,-0.016763639006558));
#12183=CARTESIAN_POINT('',(-0.0175000000005,0.,0.));
#12184=CARTESIAN_POINT('',(-0.0174999998752501,-0.000403104003887938,-0.0174953565862604));
#12185=CARTESIAN_POINT('',(-0.0175,-0.00100000000007961,-0.0129614813976545));
#12186=CARTESIAN_POINT('',(-0.0175,-0.00080103466949616,-0.0144727731273847));
#12187=CARTESIAN_POINT('',(-0.0175,-0.00060206933891271,-0.0159840648571149));
#12188=CARTESIAN_POINT('',(-0.0175,-0.00040310400832926,-0.0174953565868451));
#12189=CARTESIAN_POINT('',(-0.0175,-0.00100000000005307,-0.0129614813974363));
#12190=CARTESIAN_POINT('',(-0.0175,-0.00100000000007961,-0.0124599359095369));
#12191=CARTESIAN_POINT('',(-0.0175,-0.00100000000007961,-0.0126271177389094));
#12192=CARTESIAN_POINT('',(-0.0175,-0.00100000000007961,-0.0127942995682819));
#12193=CARTESIAN_POINT('',(-0.0175,-0.00100000000007961,-0.0129614813976545));
#12194=CARTESIAN_POINT('',(-0.0005,-0.001,-0.0127107085955));
#12195=CARTESIAN_POINT('',(-0.0175,-0.001,-0.012961481397));
#12196=CARTESIAN_POINT('',(-0.0171666666633333,-0.001,-0.012961481397));
#12197=CARTESIAN_POINT('',(-0.0168333333266667,-0.001,-0.012961481397));
#12198=CARTESIAN_POINT('',(-0.01649999999,-0.001,-0.012961481397));
#12199=CARTESIAN_POINT('',(-0.016499999995,-0.00100000000001226,-0.0129614813969069));
#12200=CARTESIAN_POINT('',(-0.01649999999,-0.001,-0.012961481397));
#12201=CARTESIAN_POINT('',(-0.00549999999333333,-0.001,-0.012961481397));
#12202=CARTESIAN_POINT('',(0.00550000000333333,-0.001,-0.012961481397));
#12203=CARTESIAN_POINT('',(0.0165,-0.001,-0.012961481397));
#12204=CARTESIAN_POINT('',(0.0165,-0.001,-0.0129614811469079));
#12205=CARTESIAN_POINT('',(0.0165,-0.001,-0.0129614811469079));
#12206=CARTESIAN_POINT('',(0.0165,-0.001,-0.0127942993626052));
#12207=CARTESIAN_POINT('',(0.0165,-0.001,-0.0126271175783026));
#12208=CARTESIAN_POINT('',(0.0165,-0.001,-0.012459935794));
#12209=CARTESIAN_POINT('',(0.0165,-1.73472347597681E-19,-0.0127315880896832));
#12210=CARTESIAN_POINT('',(0.0165,0.,0.));
#12211=CARTESIAN_POINT('',(0.0165,0.001,-0.0129614812809713));
#12212=CARTESIAN_POINT('',(0.0165,0.001,-0.0129614812809713));
#12213=CARTESIAN_POINT('',(0.0165,0.001,-0.012794299497191));
#12214=CARTESIAN_POINT('',(0.0165,0.001,-0.0126271177134107));
#12215=CARTESIAN_POINT('',(0.0165,0.001,-0.0124599359296304));
#12216=CARTESIAN_POINT('',(-0.0005,0.001,-0.0127107085955));
#12217=CARTESIAN_POINT('',(0.0165,0.001,-0.012961481397));
#12218=CARTESIAN_POINT('',(0.00550000000333333,0.001,-0.012961481397));
#12219=CARTESIAN_POINT('',(-0.00549999999333333,0.001,-0.012961481397));
#12220=CARTESIAN_POINT('',(-0.01649999999,0.001,-0.012961481397));
#12221=CARTESIAN_POINT('',(-0.016499999995,0.001,-0.0129614813969079));
#12222=CARTESIAN_POINT('',(-0.01649999999,0.001,-0.012961481397));
#12223=CARTESIAN_POINT('',(-0.0168333333266667,0.001,-0.012961481397));
#12224=CARTESIAN_POINT('',(-0.0171666666633333,0.001,-0.012961481397));
#12225=CARTESIAN_POINT('',(-0.0175,0.001,-0.012961481397));
#12226=CARTESIAN_POINT('',(-0.0175,0.00100000000002654,-0.0129614813972181));
#12227=CARTESIAN_POINT('',(-0.0175,0.001,-0.012961481397));
#12228=CARTESIAN_POINT('',(-0.0175,0.001,-0.0127942995293333));
#12229=CARTESIAN_POINT('',(-0.0175,0.001,-0.0126271176616667));
#12230=CARTESIAN_POINT('',(-0.0175,0.001,-0.012459935794));
#12231=CARTESIAN_POINT('',(-0.0175,0.002713045933,-0.0148272384280001));
#12232=CARTESIAN_POINT('',(-0.0175,0.000403103989373926,-0.0174953567308252));
#12233=CARTESIAN_POINT('',(-0.0175,0.00060206932627582,-0.0159840649531016));
#12234=CARTESIAN_POINT('',(-0.0175,0.000801034663177715,-0.014472773175378));
#12235=CARTESIAN_POINT('',(-0.0175,0.00100000000007961,-0.0129614813976545));
#12236=CARTESIAN_POINT('',(-0.0174999997505,0.000403103995825536,-0.0174953567316746));
#12237=CARTESIAN_POINT('',(-0.0175000000005,0.,0.));
#12238=CARTESIAN_POINT('',(-0.0174999998752501,0.00502298781526529,-0.0167636388750728));
#12239=CARTESIAN_POINT('',(-0.0175,0.00305426150693498,-0.0126361183371985));
#12240=CARTESIAN_POINT('',(-0.0175,0.00371050360930258,-0.0140119585166852));
#12241=CARTESIAN_POINT('',(-0.0175,0.00436674571167017,-0.0153877986961718));
#12242=CARTESIAN_POINT('',(-0.0175,0.00502298781403776,-0.0167636388756584));
#12243=CARTESIAN_POINT('',(-0.0175,0.00305426150728999,-0.0126361183374657));
#12244=CARTESIAN_POINT('',(-0.0175,0.00289927542909687,-0.0121591202348228));
#12245=CARTESIAN_POINT('',(-0.0175,0.00295093745504291,-0.0123181196022814));
#12246=CARTESIAN_POINT('',(-0.0175,0.00300259948098895,-0.01247711896974));
#12247=CARTESIAN_POINT('',(-0.0175,0.00305426150693498,-0.0126361183371985));
#12248=CARTESIAN_POINT('',(-0.0005,0.0029767684505,-0.012397619231));
#12249=CARTESIAN_POINT('',(-0.0175,0.003054261508,-0.012636118338));
#12250=CARTESIAN_POINT('',(-0.0171666666633333,0.003054261508,-0.012636118338));
#12251=CARTESIAN_POINT('',(-0.0168333333266667,0.003054261508,-0.012636118338));
#12252=CARTESIAN_POINT('',(-0.01649999999,0.003054261508,-0.012636118338));
#12253=CARTESIAN_POINT('',(-0.016499999995,0.00305426150790531,-0.0126361183378015));
#12254=CARTESIAN_POINT('',(-0.01649999999,0.003054261508,-0.012636118338));
#12255=CARTESIAN_POINT('',(-0.00549999999333333,0.003054261508,-0.012636118338));
#12256=CARTESIAN_POINT('',(0.00550000000333333,0.003054261508,-0.012636118338));
#12257=CARTESIAN_POINT('',(0.0165,0.003054261508,-0.012636118338));
#12258=CARTESIAN_POINT('',(0.0165,0.00305426143067905,-0.0126361181000306));
#12259=CARTESIAN_POINT('',(0.0165,0.00305426143067905,-0.0126361181000306));
#12260=CARTESIAN_POINT('',(0.0165,0.00300259941811937,-0.0124771187746871));
#12261=CARTESIAN_POINT('',(0.0165,0.00295093740555969,-0.0123181194493435));
#12262=CARTESIAN_POINT('',(0.0165,0.002899275393,-0.012159120124));
#12263=CARTESIAN_POINT('',(0.0165,0.0039278249665,-0.0120886022365));
#12264=CARTESIAN_POINT('',(0.0165,0.,0.));
#12265=CARTESIAN_POINT('',(0.0165,0.00495637450404248,-0.0120180842387746));
#12266=CARTESIAN_POINT('',(0.0165,0.00495637450391302,-0.0120180842388167));
#12267=CARTESIAN_POINT('',(0.0165,0.00490471249154851,-0.0118590849140078));
#12268=CARTESIAN_POINT('',(0.0165,0.00485305047918401,-0.0117000855891988));
#12269=CARTESIAN_POINT('',(0.0165,0.0048013884668195,-0.0115410862643899));
#12270=CARTESIAN_POINT('',(-0.0005,0.004878881483,-0.011779585242));
#12271=CARTESIAN_POINT('',(0.0165,0.00495637454,-0.012018084349));
#12272=CARTESIAN_POINT('',(0.00550000000333333,0.00495637454,-0.012018084349));
#12273=CARTESIAN_POINT('',(-0.00549999999333332,0.00495637454,-0.012018084349));
#12274=CARTESIAN_POINT('',(-0.01649999999,0.00495637454,-0.012018084349));
#12275=CARTESIAN_POINT('',(-0.016499999995,0.00495637453999739,-0.0120180843489919));
#12276=CARTESIAN_POINT('',(-0.01649999999,0.00495637454,-0.012018084349));
#12277=CARTESIAN_POINT('',(-0.0168333333266667,0.00495637454,-0.012018084349));
#12278=CARTESIAN_POINT('',(-0.0171666666633333,0.00495637454,-0.012018084349));
#12279=CARTESIAN_POINT('',(-0.0175,0.00495637454,-0.012018084349));
#12280=CARTESIAN_POINT('',(-0.0175,0.00495637454010061,-0.0120180843492958));
#12281=CARTESIAN_POINT('',(-0.0175,0.00495637454,-0.012018084349));
#12282=CARTESIAN_POINT('',(-0.0175,0.004904712502,-0.0118590849443333));
#12283=CARTESIAN_POINT('',(-0.0175,0.004853050464,-0.0117000855396667));
#12284=CARTESIAN_POINT('',(-0.0175,0.004801388426,-0.011541086135));
#12285=CARTESIAN_POINT('',(-0.0175,0.0073793915595,-0.0135912960505));
#12286=CARTESIAN_POINT('',(-0.0175,0.00578973722604522,-0.0165145070419431));
#12287=CARTESIAN_POINT('',(-0.0175,0.00551194966413076,-0.0150156994779245));
#12288=CARTESIAN_POINT('',(-0.0175,0.00523416210221629,-0.0135168919139059));
#12289=CARTESIAN_POINT('',(-0.0175,0.00495637454030183,-0.0120180843498873));
#12290=CARTESIAN_POINT('',(-0.0174999997505,0.00578973722878568,-0.0165145070414352));
#12291=CARTESIAN_POINT('',(-0.0175000000005,0.,0.));
#12292=CARTESIAN_POINT('',(-0.0174999998752501,0.00995739459048621,-0.0143909793923937));
#12293=CARTESIAN_POINT('',(-0.0175,0.00680955061903612,-0.0110738439744768));
#12294=CARTESIAN_POINT('',(-0.0175,0.00785883194344592,-0.0121795557798863));
#12295=CARTESIAN_POINT('',(-0.0175,0.00890811326785571,-0.0132852675852957));
#12296=CARTESIAN_POINT('',(-0.0175,0.00995739459226551,-0.0143909793907052));
#12297=CARTESIAN_POINT('',(-0.0175,0.00680955061902408,-0.0110738439746512));
#12298=CARTESIAN_POINT('',(-0.0175,0.0065147495766586,-0.0106680851532603));
#12299=CARTESIAN_POINT('',(-0.0175,0.00661301659078444,-0.0108033380936658));
#12300=CARTESIAN_POINT('',(-0.0175,0.00671128360491028,-0.0109385910340713));
#12301=CARTESIAN_POINT('',(-0.0175,0.00680955061903612,-0.0110738439744768));
#12302=CARTESIAN_POINT('',(-0.0005,0.00666215006449998,-0.010870964517));
#12303=CARTESIAN_POINT('',(-0.0175,0.00680955061899999,-0.011073843975));
#12304=CARTESIAN_POINT('',(-0.0171666666633333,0.00680955061899999,-0.011073843975));
#12305=CARTESIAN_POINT('',(-0.0168333333266667,0.00680955061899999,-0.011073843975));
#12306=CARTESIAN_POINT('',(-0.01649999999,0.00680955061899999,-0.011073843975));
#12307=CARTESIAN_POINT('',(-0.016499999995,0.00680955061879209,-0.0110738439747809));
#12308=CARTESIAN_POINT('',(-0.01649999999,0.00680955061899999,-0.011073843975));
#12309=CARTESIAN_POINT('',(-0.00549999999333334,0.00680955061899999,-0.011073843975));
#12310=CARTESIAN_POINT('',(0.00550000000333334,0.00680955061899999,-0.011073843975));
#12311=CARTESIAN_POINT('',(0.0165,0.00680955061899999,-0.011073843975));
#12312=CARTESIAN_POINT('',(0.0165,0.00680955047187945,-0.011073843772506));
#12313=CARTESIAN_POINT('',(0.0165,0.00680955047187945,-0.011073843772506));
#12314=CARTESIAN_POINT('',(0.0165,0.0067112834845863,-0.010938590868004));
#12315=CARTESIAN_POINT('',(0.0165,0.00661301649729314,-0.010803337963502));
#12316=CARTESIAN_POINT('',(0.0165,0.00651474950999999,-0.010668085059));
#12317=CARTESIAN_POINT('',(0.0165,0.0074711670585,-0.0102831792645));
#12318=CARTESIAN_POINT('',(0.0165,0.,0.));
#12319=CARTESIAN_POINT('',(0.0165,0.00842758453894735,-0.00989827337663452));
#12320=CARTESIAN_POINT('',(0.0165,0.00842758453880426,-0.00989827337673848));
#12321=CARTESIAN_POINT('',(0.0165,0.00832931755198811,-0.00976302047262217));
#12322=CARTESIAN_POINT('',(0.0165,0.00823105056517196,-0.00962776756850585));
#12323=CARTESIAN_POINT('',(0.0165,0.00813278357835582,-0.00949251466438954));
#12324=CARTESIAN_POINT('',(-0.0005,0.00828018405299999,-0.00969539401200001));
#12325=CARTESIAN_POINT('',(0.0165,0.00842758460699999,-0.00989827347000001));
#12326=CARTESIAN_POINT('',(0.00550000000333334,0.00842758460699999,-0.00989827347000001));
#12327=CARTESIAN_POINT('',(-0.00549999999333334,0.00842758460699999,-0.00989827347000001));
#12328=CARTESIAN_POINT('',(-0.01649999999,0.00842758460699999,-0.00989827347000001));
#12329=CARTESIAN_POINT('',(-0.016499999995,0.00842758460705612,-0.00989827347007726));
#12330=CARTESIAN_POINT('',(-0.01649999999,0.00842758460699999,-0.00989827347000001));
#12331=CARTESIAN_POINT('',(-0.0168333333266667,0.00842758460699999,-0.00989827347000001));
#12332=CARTESIAN_POINT('',(-0.0171666666633333,0.00842758460699999,-0.00989827347000001));
#12333=CARTESIAN_POINT('',(-0.0175,0.00842758460699999,-0.00989827347000001));
#12334=CARTESIAN_POINT('',(-0.0175,0.00842758460672372,-0.0098982734697996));
#12335=CARTESIAN_POINT('',(-0.0175,0.00842758460699999,-0.00989827347000001));
#12336=CARTESIAN_POINT('',(-0.0175,0.00832931757099999,-0.00976302049800001));
#12337=CARTESIAN_POINT('',(-0.0175,0.00823105053499999,-0.00962776752600001));
#12338=CARTESIAN_POINT('',(-0.0175,0.00813278349899999,-0.00949251455400001));
#12339=CARTESIAN_POINT('',(-0.0175,0.011024942919,-0.011024942919));
#12340=CARTESIAN_POINT('',(-0.0175,0.0106096306507946,-0.0139171023384044));
#12341=CARTESIAN_POINT('',(-0.0175,0.00988228196925343,-0.0125774927154025));
#12342=CARTESIAN_POINT('',(-0.0175,0.0091549332877123,-0.0112378830924007));
#12343=CARTESIAN_POINT('',(-0.0175,0.00842758460617116,-0.00989827346939879));
#12344=CARTESIAN_POINT('',(-0.0174999997505,0.0106096306436055,-0.0139171023423077));
#12345=CARTESIAN_POINT('',(-0.0175000000005,0.,0.));
#12346=CARTESIAN_POINT('',(-0.0174999998752501,0.0139171022121162,-0.0106096305765927));
#12347=CARTESIAN_POINT('',(-0.0175,0.00989827346939877,-0.00842758460617117));
#12348=CARTESIAN_POINT('',(-0.0175,0.0112378830495172,-0.00915493326442851));
#12349=CARTESIAN_POINT('',(-0.0175,0.0125774926296357,-0.00988228192268585));
#12350=CARTESIAN_POINT('',(-0.0175,0.0139171022097541,-0.0106096305809432));
#12351=CARTESIAN_POINT('',(-0.0175,0.00989827346959919,-0.00842758460644744));
#12352=CARTESIAN_POINT('',(-0.0175,0.00949251464684353,-0.00813278356824452));
#12353=CARTESIAN_POINT('',(-0.0175,0.00962776758769528,-0.00823105058088674));
#12354=CARTESIAN_POINT('',(-0.0175,0.00976302052854702,-0.00832931759352895));
#12355=CARTESIAN_POINT('',(-0.0175,0.00989827346939877,-0.00842758460617117));
#12356=CARTESIAN_POINT('',(-0.0005,0.009695394012,-0.00828018405299999));
#12357=CARTESIAN_POINT('',(-0.0175,0.00989827347000001,-0.00842758460699999));
#12358=CARTESIAN_POINT('',(-0.0171666666633333,0.00989827347000001,-0.00842758460699999));
#12359=CARTESIAN_POINT('',(-0.0168333333266667,0.00989827347000001,-0.00842758460699999));
#12360=CARTESIAN_POINT('',(-0.01649999999,0.00989827347000001,-0.00842758460699999));
#12361=CARTESIAN_POINT('',(-0.016499999995,0.00989827347008551,-0.00842758460704643));
#12362=CARTESIAN_POINT('',(-0.01649999999,0.00989827347000001,-0.00842758460699999));
#12363=CARTESIAN_POINT('',(-0.00549999999333333,0.00989827347000001,-0.00842758460699999));
#12364=CARTESIAN_POINT('',(0.00550000000333333,0.00989827347000001,-0.00842758460699999));
#12365=CARTESIAN_POINT('',(0.0165,0.00989827347000001,-0.00842758460699999));
#12366=CARTESIAN_POINT('',(0.0165,0.00989827326782301,-0.00842758446010981));
#12367=CARTESIAN_POINT('',(0.0165,0.00989827326782301,-0.00842758446010981));
#12368=CARTESIAN_POINT('',(0.0165,0.00976302036321534,-0.0083293174730732));
#12369=CARTESIAN_POINT('',(0.0165,0.00962776745860767,-0.0082310504860366));
#12370=CARTESIAN_POINT('',(0.0165,0.009492514554,-0.00813278349899999));
#12371=CARTESIAN_POINT('',(0.0165,0.0102831792645,-0.0074711670585));
#12372=CARTESIAN_POINT('',(0.0165,0.,0.));
#12373=CARTESIAN_POINT('',(0.0165,0.0110738438809193,-0.0068095505505698));
#12374=CARTESIAN_POINT('',(0.0165,0.0110738438809557,-0.00680955055051969));
#12375=CARTESIAN_POINT('',(0.0165,0.0109385909766482,-0.00671128356356468));
#12376=CARTESIAN_POINT('',(0.0165,0.0108033380723408,-0.00661301657660966));
#12377=CARTESIAN_POINT('',(0.0165,0.0106680851680333,-0.00651474958965464));
#12378=CARTESIAN_POINT('',(-0.0005,0.010870964517,-0.00666215006449997));
#12379=CARTESIAN_POINT('',(0.0165,0.011073843975,-0.00680955061899998));
#12380=CARTESIAN_POINT('',(0.00550000000333333,0.011073843975,-0.00680955061899998));
#12381=CARTESIAN_POINT('',(-0.00549999999333332,0.011073843975,-0.00680955061899998));
#12382=CARTESIAN_POINT('',(-0.01649999999,0.011073843975,-0.00680955061899998));
#12383=CARTESIAN_POINT('',(-0.016499999995,0.0110738439747602,-0.00680955061882576));
#12384=CARTESIAN_POINT('',(-0.01649999999,0.011073843975,-0.00680955061899998));
#12385=CARTESIAN_POINT('',(-0.0168333333266667,0.011073843975,-0.00680955061899998));
#12386=CARTESIAN_POINT('',(-0.0171666666633333,0.011073843975,-0.00680955061899998));
#12387=CARTESIAN_POINT('',(-0.0175,0.011073843975,-0.00680955061899998));
#12388=CARTESIAN_POINT('',(-0.0175,0.0110738439748256,-0.00680955061901203));
#12389=CARTESIAN_POINT('',(-0.0175,0.011073843975,-0.00680955061899998));
#12390=CARTESIAN_POINT('',(-0.0175,0.010938591003,-0.00671128358266665));
#12391=CARTESIAN_POINT('',(-0.0175,0.010803338031,-0.00661301654633331));
#12392=CARTESIAN_POINT('',(-0.0175,0.010668085059,-0.00651474950999998));
#12393=CARTESIAN_POINT('',(-0.0175,0.0135912960505,-0.0073793915595));
#12394=CARTESIAN_POINT('',(-0.0175,0.014390979497136,-0.00995739469326454));
#12395=CARTESIAN_POINT('',(-0.0175,0.0132852676562496,-0.0089081133351884));
#12396=CARTESIAN_POINT('',(-0.0175,0.0121795558153632,-0.00785883197711226));
#12397=CARTESIAN_POINT('',(-0.0175,0.0110738439744768,-0.00680955061903612));
#12398=CARTESIAN_POINT('',(-0.0174999997505,0.0143909795016971,-0.00995739468845805));
#12399=CARTESIAN_POINT('',(-0.0175000000005,0.,0.));
#12400=CARTESIAN_POINT('',(-0.0174999998752501,0.0165145068977519,-0.00578973719986344));
#12401=CARTESIAN_POINT('',(-0.0175,0.0120180843498873,-0.00495637454030183));
#12402=CARTESIAN_POINT('',(-0.0175,0.0135168918658746,-0.00523416209331421));
#12403=CARTESIAN_POINT('',(-0.0175,0.0150156993818619,-0.0055119496463266));
#12404=CARTESIAN_POINT('',(-0.0175,0.0165145068978492,-0.00578973719933899));
#12405=CARTESIAN_POINT('',(-0.0175,0.0120180843495915,-0.00495637454020122));
#12406=CARTESIAN_POINT('',(-0.0175,0.0115410862463895,-0.00480138846209655));
#12407=CARTESIAN_POINT('',(-0.0175,0.0117000856142221,-0.00485305048816498));
#12408=CARTESIAN_POINT('',(-0.0175,0.0118590849820547,-0.0049047125142334));
#12409=CARTESIAN_POINT('',(-0.0175,0.0120180843498873,-0.00495637454030183));
#12410=CARTESIAN_POINT('',(-0.0005,0.011779585242,-0.004878881483));
#12411=CARTESIAN_POINT('',(-0.0175,0.012018084349,-0.00495637454));
#12412=CARTESIAN_POINT('',(-0.0171666666633333,0.012018084349,-0.00495637454));
#12413=CARTESIAN_POINT('',(-0.0168333333266667,0.012018084349,-0.00495637454));
#12414=CARTESIAN_POINT('',(-0.01649999999,0.012018084349,-0.00495637454));
#12415=CARTESIAN_POINT('',(-0.016499999995,0.0120180843489915,-0.00495637453999843));
#12416=CARTESIAN_POINT('',(-0.01649999999,0.012018084349,-0.00495637454));
#12417=CARTESIAN_POINT('',(-0.00549999999333334,0.012018084349,-0.00495637454));
#12418=CARTESIAN_POINT('',(0.00550000000333334,0.012018084349,-0.00495637454));
#12419=CARTESIAN_POINT('',(0.0165,0.012018084349,-0.00495637454));
#12420=CARTESIAN_POINT('',(0.0165,0.0120180841112278,-0.00495637446274314));
#12421=CARTESIAN_POINT('',(0.0165,0.0120180841112278,-0.00495637446274314));
#12422=CARTESIAN_POINT('',(0.0165,0.0118590847858185,-0.00490471245049542));
#12423=CARTESIAN_POINT('',(0.0165,0.0117000854604093,-0.00485305043824771));
#12424=CARTESIAN_POINT('',(0.0165,0.011541086135,-0.004801388426));
#12425=CARTESIAN_POINT('',(0.0165,0.0120886022365,-0.00392782496650001));
#12426=CARTESIAN_POINT('',(0.0165,0.,0.));
#12427=CARTESIAN_POINT('',(0.0165,0.0126361182276936,-0.0030542614722702));
#12428=CARTESIAN_POINT('',(0.0165,0.012636118227661,-0.00305426147237052));
#12429=CARTESIAN_POINT('',(0.0165,0.0124771189027977,-0.00300259945998833));
#12430=CARTESIAN_POINT('',(0.0165,0.0123181195779343,-0.00295093744760614));
#12431=CARTESIAN_POINT('',(0.0165,0.0121591202530709,-0.00289927543522395));
#12432=CARTESIAN_POINT('',(-0.0005,0.012397619231,-0.0029767684505));
#12433=CARTESIAN_POINT('',(0.0165,0.012636118338,-0.003054261508));
#12434=CARTESIAN_POINT('',(0.00550000000333333,0.012636118338,-0.003054261508));
#12435=CARTESIAN_POINT('',(-0.00549999999333333,0.012636118338,-0.003054261508));
#12436=CARTESIAN_POINT('',(-0.01649999999,0.012636118338,-0.003054261508));
#12437=CARTESIAN_POINT('',(-0.016499999995,0.0126361183377947,-0.00305426150793331));
#12438=CARTESIAN_POINT('',(-0.01649999999,0.012636118338,-0.003054261508));
#12439=CARTESIAN_POINT('',(-0.0168333333266667,0.012636118338,-0.003054261508));
#12440=CARTESIAN_POINT('',(-0.0171666666633333,0.012636118338,-0.003054261508));
#12441=CARTESIAN_POINT('',(-0.0175,0.012636118338,-0.003054261508));
#12442=CARTESIAN_POINT('',(-0.0175,0.0126361183377328,-0.003054261507645));
#12443=CARTESIAN_POINT('',(-0.0175,0.012636118338,-0.003054261508));
#12444=CARTESIAN_POINT('',(-0.0175,0.0124771189333333,-0.00300259946966667));
#12445=CARTESIAN_POINT('',(-0.0175,0.0123181195286667,-0.00295093743133333));
#12446=CARTESIAN_POINT('',(-0.0175,0.012159120124,-0.002899275393));
#12447=CARTESIAN_POINT('',(-0.0175,0.014827238428,-0.002713045933));
#12448=CARTESIAN_POINT('',(-0.0175,0.0167636390080186,-0.00502298787717037));
#12449=CARTESIAN_POINT('',(-0.0175,0.0153877987844119,-0.00436674575375858));
#12450=CARTESIAN_POINT('',(-0.0175,0.0140119585608052,-0.00371050363034678));
#12451=CARTESIAN_POINT('',(-0.0175,0.0126361183371985,-0.00305426150693499));
#12452=CARTESIAN_POINT('',(-0.0174999997505,0.0167636390075883,-0.00502298787807265));
#12453=CARTESIAN_POINT('',(-0.0175000000005,0.,0.));
#12454=CARTESIAN_POINT('',(-0.0174999998752501,0.0174953565861002,-0.000403104010841439));
#12455=CARTESIAN_POINT('',(-0.0175,0.0129614813976545,-0.00100000000007961));
#12456=CARTESIAN_POINT('',(-0.0175,0.0144727731270322,-0.000801034669542563));
#12457=CARTESIAN_POINT('',(-0.0175,0.01598406485641,-0.000602069339005512));
#12458=CARTESIAN_POINT('',(-0.0175,0.0174953565857878,-0.000403104008468461));
#12459=CARTESIAN_POINT('',(-0.0175,0.0129614813974363,-0.00100000000005307));
#12460=CARTESIAN_POINT('',(-0.0175,0.0124599359091394,-0.00100000000007962));
#12461=CARTESIAN_POINT('',(-0.0175,0.0126271177386444,-0.00100000000007962));
#12462=CARTESIAN_POINT('',(-0.0175,0.0127942995681494,-0.00100000000007962));
#12463=CARTESIAN_POINT('',(-0.0175,0.0129614813976545,-0.00100000000007962));
#12464=CARTESIAN_POINT('',(-0.0005,0.0127107085955,-0.001));
#12465=CARTESIAN_POINT('',(-0.0175,0.012961481397,-0.001));
#12466=CARTESIAN_POINT('',(-0.0171666666633333,0.012961481397,-0.001));
#12467=CARTESIAN_POINT('',(-0.0168333333266667,0.012961481397,-0.001));
#12468=CARTESIAN_POINT('',(-0.01649999999,0.012961481397,-0.001));
#12469=CARTESIAN_POINT('',(-0.016499999995,0.0129614813969069,-0.00100000000001226));
#12470=CARTESIAN_POINT('',(-0.01649999999,0.012961481397,-0.001));
#12471=CARTESIAN_POINT('',(-0.005500000035,0.012961481397,-0.001));
#12472=CARTESIAN_POINT('',(0.00549999992,0.012961481397,-0.001));
#12473=CARTESIAN_POINT('',(0.016499999875,0.012961481397,-0.001));
#12474=CARTESIAN_POINT('',(-0.0215,0.,-3.07046055247895E-18));
#12475=CARTESIAN_POINT('',(-0.0215,0.,0.));
#12476=CARTESIAN_POINT('',(-0.0215,0.,0.0175));
#12477=CARTESIAN_POINT('',(-0.019981842228,0.,0.));
#12478=CARTESIAN_POINT('',(-0.0165,0.,0.));
#12479=CARTESIAN_POINT('',(-0.017,0.0152284190645,0.000701551994));
#12480=CARTESIAN_POINT('',(-0.0174999998755,0.017495356732,0.000403103988));
#12481=CARTESIAN_POINT('',(-0.017166666667,0.017495356732,0.000403103988));
#12482=CARTESIAN_POINT('',(-0.0168333334585,0.017495356732,0.000403103988));
#12483=CARTESIAN_POINT('',(-0.01650000025,0.017495356732,0.000403103988));
#12484=CARTESIAN_POINT('',(-0.01650000025,0.0174953567319272,0.000403103988009585));
#12485=CARTESIAN_POINT('',(-0.0165,0.0174953567319272,0.000403103988009584));
#12486=CARTESIAN_POINT('',(-0.0165,0.0159840649536181,0.000602069325339723));
#12487=CARTESIAN_POINT('',(-0.0165,0.0144727731753091,0.000801034662669862));
#12488=CARTESIAN_POINT('',(-0.0165,0.012961481397,0.001));
#12489=CARTESIAN_POINT('',(-0.017,0.014699878673,0.004038624693));
#12490=CARTESIAN_POINT('',(-0.0165,0.016763639008,0.005022987878));
#12491=CARTESIAN_POINT('',(-0.0168333333333333,0.016763639008,0.005022987878));
#12492=CARTESIAN_POINT('',(-0.0171666666666667,0.016763639008,0.005022987878));
#12493=CARTESIAN_POINT('',(-0.0175,0.016763639008,0.005022987878));
#12494=CARTESIAN_POINT('',(-0.0165,0.0167636387823537,0.00502298777037222));
#12495=CARTESIAN_POINT('',(-0.0165,0.012636118338,0.003054261508));
#12496=CARTESIAN_POINT('',(-0.0165,0.0140119584861179,0.00371050359545741));
#12497=CARTESIAN_POINT('',(-0.0165,0.0153877986342358,0.00436674568291482));
#12498=CARTESIAN_POINT('',(-0.0165,0.0167636387823537,0.00502298777037223));
#12499=CARTESIAN_POINT('',(-0.034017463007,0.,0.));
#12500=CARTESIAN_POINT('',(-0.0174999998755,-0.017495356732,-0.000403103988));
#12501=CARTESIAN_POINT('',(-0.017166666667,-0.017495356732,-0.000403103988));
#12502=CARTESIAN_POINT('',(-0.0168333334585,-0.017495356732,-0.000403103988));
#12503=CARTESIAN_POINT('',(-0.01650000025,-0.017495356732,-0.000403103988));
#12504=CARTESIAN_POINT('',(-0.01650000025,-0.0174953567319272,-0.000403103988009585));
#12505=CARTESIAN_POINT('',(-0.0165,0.,0.));
#12506=CARTESIAN_POINT('',(-0.016500000125,-0.01749535673194,0.000403103987454157));
#12507=CARTESIAN_POINT('',(-0.0174999997505,-0.01749535673188,0.000403103986908313));
#12508=CARTESIAN_POINT('',(-0.0171666665836667,-0.01749535673188,0.000403103986908313));
#12509=CARTESIAN_POINT('',(-0.0168333334168333,-0.01749535673188,0.000403103986908313));
#12510=CARTESIAN_POINT('',(-0.01650000025,-0.01749535673188,0.000403103986908313));
#12511=CARTESIAN_POINT('',(-0.01650000025,-0.0167636390090209,0.00502298787329154));
#12512=CARTESIAN_POINT('',(-0.0168333334168333,-0.0167636390090209,0.00502298787329154));
#12513=CARTESIAN_POINT('',(-0.0171666665836667,-0.0167636390090209,0.00502298787329154));
#12514=CARTESIAN_POINT('',(-0.0174999997505,-0.0167636390090209,0.00502298787329154));
#12515=CARTESIAN_POINT('',(-0.0165,-0.0167636390078825,0.00502298787774123));
#12516=CARTESIAN_POINT('',(-0.0165,0.,0.));
#12517=CARTESIAN_POINT('',(-0.016500000125,-0.0165145070431931,0.0057897372241842));
#12518=CARTESIAN_POINT('',(-0.0174999997505,-0.0165145070443862,0.00578973722036841));
#12519=CARTESIAN_POINT('',(-0.0171666665836667,-0.0165145070443862,0.00578973722036841));
#12520=CARTESIAN_POINT('',(-0.0168333334168333,-0.0165145070443862,0.00578973722036841));
#12521=CARTESIAN_POINT('',(-0.01650000025,-0.0165145070443862,0.00578973722036841));
#12522=CARTESIAN_POINT('',(-0.01650000025,-0.0143909794945797,0.00995739469874462));
#12523=CARTESIAN_POINT('',(-0.0168333334168333,-0.0143909794945797,0.00995739469874462));
#12524=CARTESIAN_POINT('',(-0.0171666665836667,-0.0143909794945797,0.00995739469874462));
#12525=CARTESIAN_POINT('',(-0.0174999997505,-0.0143909794945797,0.00995739469874462));
#12526=CARTESIAN_POINT('',(-0.0165,-0.0143909794950452,0.00995739469767118));
#12527=CARTESIAN_POINT('',(-0.0165,0.,0.));
#12528=CARTESIAN_POINT('',(-0.016500000125,-0.0139171023380528,0.0106096306492146));
#12529=CARTESIAN_POINT('',(-0.0174999997505,-0.0139171023371057,0.0106096306504292));
#12530=CARTESIAN_POINT('',(-0.0171666665836667,-0.0139171023371057,0.0106096306504292));
#12531=CARTESIAN_POINT('',(-0.0168333334168333,-0.0139171023371057,0.0106096306504292));
#12532=CARTESIAN_POINT('',(-0.01650000025,-0.0139171023371057,0.0106096306504292));
#12533=CARTESIAN_POINT('',(-0.01650000025,-0.0106096306475748,0.0139171023392818));
#12534=CARTESIAN_POINT('',(-0.0168333334168333,-0.0106096306475748,0.0139171023392818));
#12535=CARTESIAN_POINT('',(-0.0171666665836667,-0.0106096306475748,0.0139171023392818));
#12536=CARTESIAN_POINT('',(-0.0174999997505,-0.0106096306475748,0.0139171023392818));
#12537=CARTESIAN_POINT('',(-0.0165,-0.0106096306460396,0.0139171023404521));
#12538=CARTESIAN_POINT('',(-0.0165,0.,0.));
#12539=CARTESIAN_POINT('',(-0.016500000125,-0.00995739469439649,0.014390979497311));
#12540=CARTESIAN_POINT('',(-0.0174999997505,-0.00995739469579297,0.014390979496622));
#12541=CARTESIAN_POINT('',(-0.0171666665836667,-0.00995739469579297,0.014390979496622));
#12542=CARTESIAN_POINT('',(-0.0168333334168333,-0.00995739469579297,0.014390979496622));
#12543=CARTESIAN_POINT('',(-0.01650000025,-0.00995739469579297,0.014390979496622));
#12544=CARTESIAN_POINT('',(-0.01650000025,-0.00578973723349574,0.0165145070397839));
#12545=CARTESIAN_POINT('',(-0.0168333334168333,-0.00578973723349574,0.0165145070397839));
#12546=CARTESIAN_POINT('',(-0.0171666665836667,-0.00578973723349574,0.0165145070397839));
#12547=CARTESIAN_POINT('',(-0.0174999997505,-0.00578973723349574,0.0165145070397839));
#12548=CARTESIAN_POINT('',(-0.0165,-0.00578973722868356,0.0165145070416157));
#12549=CARTESIAN_POINT('',(-0.0165,0.,0.));
#12550=CARTESIAN_POINT('',(-0.016500000125,-0.00502298787392663,0.0167636390090256));
#12551=CARTESIAN_POINT('',(-0.0174999997505,-0.00502298786985327,0.0167636390100511));
#12552=CARTESIAN_POINT('',(-0.0171666665836667,-0.00502298786985327,0.0167636390100511));
#12553=CARTESIAN_POINT('',(-0.0168333334168333,-0.00502298786985327,0.0167636390100511));
#12554=CARTESIAN_POINT('',(-0.01650000025,-0.00502298786985327,0.0167636390100511));
#12555=CARTESIAN_POINT('',(-0.01650000025,-0.000403103983319961,0.0174953567319627));
#12556=CARTESIAN_POINT('',(-0.0168333334168333,-0.000403103983319961,0.0174953567319627));
#12557=CARTESIAN_POINT('',(-0.0171666665836667,-0.000403103983319961,0.0174953567319627));
#12558=CARTESIAN_POINT('',(-0.0174999997505,-0.000403103983319961,0.0174953567319627));
#12559=CARTESIAN_POINT('',(-0.0165,-0.000403103982389193,0.0174953567319841));
#12560=CARTESIAN_POINT('',(-0.0165,0.,0.));
#12561=CARTESIAN_POINT('',(-0.0165000001875,0.000403103989248338,0.0174953567318987));
#12562=CARTESIAN_POINT('',(-0.0174999997505,0.000403103990496676,0.0174953567317973));
#12563=CARTESIAN_POINT('',(-0.0171666665836667,0.000403103990496676,0.0174953567317973));
#12564=CARTESIAN_POINT('',(-0.0168333334168333,0.000403103990496676,0.0174953567317973));
#12565=CARTESIAN_POINT('',(-0.01650000025,0.000403103990496676,0.0174953567317973));
#12566=CARTESIAN_POINT('',(-0.01650000025,0.00502298787672982,0.0167636390079906));
#12567=CARTESIAN_POINT('',(-0.0168333334168333,0.00502298787672982,0.0167636390079906));
#12568=CARTESIAN_POINT('',(-0.0171666665836667,0.00502298787672982,0.0167636390079906));
#12569=CARTESIAN_POINT('',(-0.0174999997505,0.00502298787672982,0.0167636390079906));
#12570=CARTESIAN_POINT('',(-0.0165,0.005022987879379,0.0167636390071969));
#12571=CARTESIAN_POINT('',(-0.0165,0.,0.));
#12572=CARTESIAN_POINT('',(-0.016500000125,0.0057897372258778,0.0165145070425994));
#12573=CARTESIAN_POINT('',(-0.0174999997505,0.00578973722375559,0.0165145070431987));
#12574=CARTESIAN_POINT('',(-0.0171666665836667,0.00578973722375559,0.0165145070431987));
#12575=CARTESIAN_POINT('',(-0.0168333334168333,0.00578973722375559,0.0165145070431987));
#12576=CARTESIAN_POINT('',(-0.01650000025,0.00578973722375559,0.0165145070431987));
#12577=CARTESIAN_POINT('',(-0.01650000025,0.00995739468730528,0.0143909795024948));
#12578=CARTESIAN_POINT('',(-0.0168333334168333,0.00995739468730528,0.0143909795024948));
#12579=CARTESIAN_POINT('',(-0.0171666665836667,0.00995739468730528,0.0143909795024948));
#12580=CARTESIAN_POINT('',(-0.0174999997505,0.00995739468730528,0.0143909795024948));
#12581=CARTESIAN_POINT('',(-0.0165,0.00995739469211033,0.0143909794991701));
#12582=CARTESIAN_POINT('',(-0.0165,0.,0.));
#12583=CARTESIAN_POINT('',(-0.016500000125,0.0106096306506418,0.0139171023369648));
#12584=CARTESIAN_POINT('',(-0.0174999997505,0.0106096306532837,0.0139171023349296));
#12585=CARTESIAN_POINT('',(-0.0171666665836667,0.0106096306532837,0.0139171023349296));
#12586=CARTESIAN_POINT('',(-0.0168333334168333,0.0106096306532837,0.0139171023349296));
#12587=CARTESIAN_POINT('',(-0.01650000025,0.0106096306532837,0.0139171023349296));
#12588=CARTESIAN_POINT('',(-0.01650000025,0.0139171023414578,0.0106096306447203));
#12589=CARTESIAN_POINT('',(-0.0168333334168333,0.0139171023414578,0.0106096306447203));
#12590=CARTESIAN_POINT('',(-0.0171666665836667,0.0139171023414578,0.0106096306447203));
#12591=CARTESIAN_POINT('',(-0.0174999997505,0.0139171023414578,0.0106096306447203));
#12592=CARTESIAN_POINT('',(-0.0165,0.0139171023415401,0.0106096306446124));
#12593=CARTESIAN_POINT('',(-0.0165,0.,0.));
#12594=CARTESIAN_POINT('',(-0.016500000125,0.0143909794983321,0.00995739469292067));
#12595=CARTESIAN_POINT('',(-0.0174999997505,0.0143909794986643,0.00995739469284135));
#12596=CARTESIAN_POINT('',(-0.0171666665836667,0.0143909794986643,0.00995739469284135));
#12597=CARTESIAN_POINT('',(-0.0168333334168333,0.0143909794986643,0.00995739469284135));
#12598=CARTESIAN_POINT('',(-0.01650000025,0.0143909794986643,0.00995739469284135));
#12599=CARTESIAN_POINT('',(-0.01650000025,0.0165145070409714,0.00578973723010854));
#12600=CARTESIAN_POINT('',(-0.0168333334168333,0.0165145070409714,0.00578973723010854));
#12601=CARTESIAN_POINT('',(-0.0171666665836667,0.0165145070409714,0.00578973723010854));
#12602=CARTESIAN_POINT('',(-0.0174999997505,0.0165145070409714,0.00578973723010854));
#12603=CARTESIAN_POINT('',(-0.0165,0.0165145070420736,0.00578973722696479));
#12604=CARTESIAN_POINT('',(-0.0165,0.,0.));
#12605=CARTESIAN_POINT('',(-0.0165,0.,0.));
#12606=CARTESIAN_POINT('',(-0.016500000125,0.0174953567318573,-0.000403103991042516));
#12607=CARTESIAN_POINT('',(-0.0174999997505,0.0174953567317146,-0.000403103994085063));
#12608=CARTESIAN_POINT('',(-0.0171666665836667,0.0174953567317146,-0.000403103994085063));
#12609=CARTESIAN_POINT('',(-0.0168333334168333,0.0174953567317146,-0.000403103994085063));
#12610=CARTESIAN_POINT('',(-0.01650000025,0.0174953567317146,-0.000403103994085063));
#12611=CARTESIAN_POINT('',(-0.01650000025,0.0167636390069604,-0.00502298788016813));
#12612=CARTESIAN_POINT('',(-0.0168333334168333,0.0167636390069604,-0.00502298788016813));
#12613=CARTESIAN_POINT('',(-0.0171666665836667,0.0167636390069604,-0.00502298788016813));
#12614=CARTESIAN_POINT('',(-0.0174999997505,0.0167636390069604,-0.00502298788016813));
#12615=CARTESIAN_POINT('',(-0.0165,0.0167636390066817,-0.00502298788109814));
#12616=CARTESIAN_POINT('',(-0.0165,0.,0.));
#12617=CARTESIAN_POINT('',(-0.016500000125,0.0165145070420056,-0.00578973722757139));
#12618=CARTESIAN_POINT('',(-0.0174999997505,0.0165145070420112,-0.0057897372271428));
#12619=CARTESIAN_POINT('',(-0.0171666665836667,0.0165145070420112,-0.0057897372271428));
#12620=CARTESIAN_POINT('',(-0.0168333334168333,0.0165145070420112,-0.0057897372271428));
#12621=CARTESIAN_POINT('',(-0.01650000025,0.0165145070420112,-0.0057897372271428));
#12622=CARTESIAN_POINT('',(-0.01650000025,0.0143909795004525,-0.00995739469025694));
#12623=CARTESIAN_POINT('',(-0.0168333334168333,0.0143909795004525,-0.00995739469025694));
#12624=CARTESIAN_POINT('',(-0.0171666665836667,0.0143909795004525,-0.00995739469025694));
#12625=CARTESIAN_POINT('',(-0.0174999997505,0.0143909795004525,-0.00995739469025694));
#12626=CARTESIAN_POINT('',(-0.0165,0.0143909794979816,-0.00995739469342733));
#12627=CARTESIAN_POINT('',(-0.0165,0.,0.));
#12628=CARTESIAN_POINT('',(-0.016500000125,0.0139171023411816,-0.0106096306451105));
#12629=CARTESIAN_POINT('',(-0.0174999997505,0.0139171023433632,-0.010609630642221));
#12630=CARTESIAN_POINT('',(-0.0171666665836667,0.0139171023433632,-0.010609630642221));
#12631=CARTESIAN_POINT('',(-0.0168333334168333,0.0139171023433632,-0.010609630642221));
#12632=CARTESIAN_POINT('',(-0.01650000025,0.0139171023433632,-0.010609630642221));
#12633=CARTESIAN_POINT('',(-0.01650000025,0.0106096306418659,-0.0139171023436339));
#12634=CARTESIAN_POINT('',(-0.0168333334168333,0.0106096306418659,-0.0139171023436339));
#12635=CARTESIAN_POINT('',(-0.0171666665836667,0.0106096306418659,-0.0139171023436339));
#12636=CARTESIAN_POINT('',(-0.0174999997505,0.0106096306418659,-0.0139171023436339));
#12637=CARTESIAN_POINT('',(-0.0165,0.0106096306431852,-0.0139171023426282));
#12638=CARTESIAN_POINT('',(-0.0165,0.,0.));
#12639=CARTESIAN_POINT('',(-0.016500000125,0.00995739469144485,-0.0143909794993533));
#12640=CARTESIAN_POINT('',(-0.0174999997505,0.00995739468988968,-0.0143909795007066));
#12641=CARTESIAN_POINT('',(-0.0171666665836667,0.00995739468988968,-0.0143909795007066));
#12642=CARTESIAN_POINT('',(-0.0168333334168333,0.00995739468988968,-0.0143909795007066));
#12643=CARTESIAN_POINT('',(-0.01650000025,0.00995739468988968,-0.0143909795007066));
#12644=CARTESIAN_POINT('',(-0.01650000025,0.00578973722672135,-0.0165145070421589));
#12645=CARTESIAN_POINT('',(-0.0168333334168333,0.00578973722672135,-0.0165145070421589));
#12646=CARTESIAN_POINT('',(-0.0171666665836667,0.00578973722672135,-0.0165145070421589));
#12647=CARTESIAN_POINT('',(-0.0174999997505,0.00578973722672135,-0.0165145070421589));
#12648=CARTESIAN_POINT('',(-0.0165,0.00578973722527119,-0.0165145070426674));
#12649=CARTESIAN_POINT('',(-0.0165,0.,0.));
#12650=CARTESIAN_POINT('',(-0.016500000125,0.00502298787887017,-0.0167636390075443));
#12651=CARTESIAN_POINT('',(-0.0174999997505,0.00502298787974032,-0.0167636390070886));
#12652=CARTESIAN_POINT('',(-0.0171666665836667,0.00502298787974032,-0.0167636390070886));
#12653=CARTESIAN_POINT('',(-0.0168333334168333,0.00502298787974032,-0.0167636390070886));
#12654=CARTESIAN_POINT('',(-0.01650000025,0.00502298787974032,-0.0167636390070886));
#12655=CARTESIAN_POINT('',(-0.01650000025,0.000403103993638577,-0.0174953567317249));
#12656=CARTESIAN_POINT('',(-0.0168333334168333,0.000403103993638577,-0.0174953567317249));
#12657=CARTESIAN_POINT('',(-0.0171666665836667,0.000403103993638577,-0.0174953567317249));
#12658=CARTESIAN_POINT('',(-0.0174999997505,0.000403103993638577,-0.0174953567317249));
#12659=CARTESIAN_POINT('',(-0.0165,0.000403103988632388,-0.0174953567319128));
#12660=CARTESIAN_POINT('',(-0.0165,0.,0.));
#12661=CARTESIAN_POINT('',(-0.016500000125,-0.000403103984089013,-0.0174953567320176));
#12662=CARTESIAN_POINT('',(-0.0174999997505,-0.000403103980178063,-0.0174953567320351));
#12663=CARTESIAN_POINT('',(-0.0171666665836667,-0.000403103980178063,-0.0174953567320351));
#12664=CARTESIAN_POINT('',(-0.0168333334168333,-0.000403103980178063,-0.0174953567320351));
#12665=CARTESIAN_POINT('',(-0.01650000025,-0.000403103980178063,-0.0174953567320351));
#12666=CARTESIAN_POINT('',(-0.01650000025,-0.00502298788360641,-0.0167636390059302));
#12667=CARTESIAN_POINT('',(-0.0168333334168333,-0.00502298788360641,-0.0167636390059302));
#12668=CARTESIAN_POINT('',(-0.0171666665836667,-0.00502298788360641,-0.0167636390059302));
#12669=CARTESIAN_POINT('',(-0.0174999997505,-0.00502298788360641,-0.0167636390059302));
#12670=CARTESIAN_POINT('',(-0.0165,-0.00502298788281727,-0.0167636390061666));
#12671=CARTESIAN_POINT('',(-0.0165,0.,0.));
#12672=CARTESIAN_POINT('',(-0.016500000125,-0.00578973722926497,-0.0165145070414119));
#12673=CARTESIAN_POINT('',(-0.0174999997505,-0.00578973723052998,-0.0165145070408237));
#12674=CARTESIAN_POINT('',(-0.0171666665836667,-0.00578973723052998,-0.0165145070408237));
#12675=CARTESIAN_POINT('',(-0.0168333334168333,-0.00578973723052998,-0.0165145070408237));
#12676=CARTESIAN_POINT('',(-0.01650000025,-0.00578973723052998,-0.0165145070408237));
#12677=CARTESIAN_POINT('',(-0.01650000025,-0.00995739469320859,-0.0143909794984102));
#12678=CARTESIAN_POINT('',(-0.0168333334168333,-0.00995739469320859,-0.0143909794984102));
#12679=CARTESIAN_POINT('',(-0.0171666665836667,-0.00995739469320859,-0.0143909794984102));
#12680=CARTESIAN_POINT('',(-0.0174999997505,-0.00995739469320859,-0.0143909794984102));
#12681=CARTESIAN_POINT('',(-0.0165,-0.00995739469490315,-0.0143909794969604));
#12682=CARTESIAN_POINT('',(-0.0165,0.,0.));
#12683=CARTESIAN_POINT('',(-0.016500000125,-0.0106096306465377,-0.0139171023400936));
#12684=CARTESIAN_POINT('',(-0.0174999997505,-0.0106096306450755,-0.0139171023411871));
#12685=CARTESIAN_POINT('',(-0.0171666665836667,-0.0106096306450755,-0.0139171023411871));
#12686=CARTESIAN_POINT('',(-0.0168333334168333,-0.0106096306450755,-0.0139171023411871));
#12687=CARTESIAN_POINT('',(-0.01650000025,-0.0106096306450755,-0.0139171023411871));
#12688=CARTESIAN_POINT('',(-0.01650000025,-0.0139171023352004,-0.0106096306529285));
#12689=CARTESIAN_POINT('',(-0.0168333334168333,-0.0139171023352004,-0.0106096306529285));
#12690=CARTESIAN_POINT('',(-0.0171666665836667,-0.0139171023352004,-0.0106096306529285));
#12691=CARTESIAN_POINT('',(-0.0174999997505,-0.0139171023352004,-0.0106096306529285));
#12692=CARTESIAN_POINT('',(-0.0165,-0.0139171023384264,-0.0106096306487246));
#12693=CARTESIAN_POINT('',(-0.0165,0.,0.));
#12694=CARTESIAN_POINT('',(-0.016500000125,-0.0143909795003744,-0.00995739468996904));
#12695=CARTESIAN_POINT('',(-0.0174999997505,-0.0143909795027489,-0.00995739468693804));
#12696=CARTESIAN_POINT('',(-0.0171666665836667,-0.0143909795027489,-0.00995739468693804));
#12697=CARTESIAN_POINT('',(-0.0168333334168333,-0.0143909795027489,-0.00995739468693804));
#12698=CARTESIAN_POINT('',(-0.01650000025,-0.0143909795027489,-0.00995739468693804));
#12699=CARTESIAN_POINT('',(-0.01650000025,-0.0165145070433464,-0.00578973722333416));
#12700=CARTESIAN_POINT('',(-0.0168333334168333,-0.0165145070433464,-0.00578973722333416));
#12701=CARTESIAN_POINT('',(-0.0171666665836667,-0.0165145070433464,-0.00578973722333416));
#12702=CARTESIAN_POINT('',(-0.0174999997505,-0.0165145070433464,-0.00578973722333416));
#12703=CARTESIAN_POINT('',(-0.0165,-0.0165145070432611,-0.00578973722357761));
#12704=CARTESIAN_POINT('',(-0.0165,0.,0.));
#12705=CARTESIAN_POINT('',(-0.016500000125,-0.0167636390080594,-0.00502298787715103));
#12706=CARTESIAN_POINT('',(-0.0174999997505,-0.0167636390081188,-0.00502298787630204));
#12707=CARTESIAN_POINT('',(-0.0171666665836667,-0.0167636390081188,-0.00502298787630204));
#12708=CARTESIAN_POINT('',(-0.0168333334168333,-0.0167636390081188,-0.00502298787630204));
#12709=CARTESIAN_POINT('',(-0.01650000025,-0.0167636390081188,-0.00502298787630204));
#12710=CARTESIAN_POINT('',(-0.018,0.,0.));
#12711=CARTESIAN_POINT('',(-0.018,0.,0.0175));
#12712=CARTESIAN_POINT('',(-0.019981842228,0.,0.));
#12713=CARTESIAN_POINT('',(-0.0165,0.,0.));
#12714=CARTESIAN_POINT('',(-0.017,0.0142662956955,0.005373055884));
#12715=CARTESIAN_POINT('',(-0.0165,0.016514507042,0.005789737228));
#12716=CARTESIAN_POINT('',(-0.0165,0.0150156994776667,0.00551194966533333));
#12717=CARTESIAN_POINT('',(-0.0165,0.0135168919133333,0.00523416210266667));
#12718=CARTESIAN_POINT('',(-0.0165,0.012018084349,0.00495637454));
#12719=CARTESIAN_POINT('',(-0.017,0.0127324117365,0.008383472656));
#12720=CARTESIAN_POINT('',(-0.0165,0.011073843975,0.006809550619));
#12721=CARTESIAN_POINT('',(-0.0165,0.012179555816,0.007858831977));
#12722=CARTESIAN_POINT('',(-0.0165,0.013285267657,0.008908113335));
#12723=CARTESIAN_POINT('',(-0.0165,0.014390979498,0.009957394693));
#12724=CARTESIAN_POINT('',(-0.019981842228,0.,0.));
#12725=CARTESIAN_POINT('',(-0.0165,0.,0.));
#12726=CARTESIAN_POINT('',(-0.017,0.0119076879045,0.00951860762750001));
#12727=CARTESIAN_POINT('',(-0.0165,0.013917102339,0.010609630648));
#12728=CARTESIAN_POINT('',(-0.0165,0.012577492716,0.00988228196766668));
#12729=CARTESIAN_POINT('',(-0.0165,0.011237883093,0.00915493328733334));
#12730=CARTESIAN_POINT('',(-0.0165,0.00989827347,0.00842758460700001));
#12731=CARTESIAN_POINT('',(-0.017,0.00951860762750001,0.0119076879045));
#12732=CARTESIAN_POINT('',(-0.0165,0.00842758460700001,0.00989827347));
#12733=CARTESIAN_POINT('',(-0.0165,0.00915493328724936,0.0112378830928453));
#12734=CARTESIAN_POINT('',(-0.0165,0.00988228196749871,0.0125774927156907));
#12735=CARTESIAN_POINT('',(-0.0165,0.0106096306477481,0.013917102338536));
#12736=CARTESIAN_POINT('',(-0.019981842228,0.,0.));
#12737=CARTESIAN_POINT('',(-0.0165,0.,0.));
#12738=CARTESIAN_POINT('',(-0.017,0.008383472656,0.0127324117365));
#12739=CARTESIAN_POINT('',(-0.0165,0.009957394693,0.014390979498));
#12740=CARTESIAN_POINT('',(-0.0165,0.008908113335,0.013285267657));
#12741=CARTESIAN_POINT('',(-0.0165,0.007858831977,0.012179555816));
#12742=CARTESIAN_POINT('',(-0.0165,0.006809550619,0.011073843975));
#12743=CARTESIAN_POINT('',(-0.017,0.005373055884,0.0142662956955));
#12744=CARTESIAN_POINT('',(-0.0165,0.00495637454,0.012018084349));
#12745=CARTESIAN_POINT('',(-0.0165,0.00523416210266667,0.0135168919133333));
#12746=CARTESIAN_POINT('',(-0.0165,0.00551194966533333,0.0150156994776667));
#12747=CARTESIAN_POINT('',(-0.0165,0.005789737228,0.016514507042));
#12748=CARTESIAN_POINT('',(-0.019981842228,0.,0.));
#12749=CARTESIAN_POINT('',(-0.0165,0.,0.));
#12750=CARTESIAN_POINT('',(-0.017,0.004038624693,0.014699878673));
#12751=CARTESIAN_POINT('',(-0.0165,0.005022987878,0.016763639008));
#12752=CARTESIAN_POINT('',(-0.0165,0.00436674575466666,0.0153877987846667));
#12753=CARTESIAN_POINT('',(-0.0165,0.00371050363133333,0.0140119585613333));
#12754=CARTESIAN_POINT('',(-0.0165,0.003054261508,0.012636118338));
#12755=CARTESIAN_POINT('',(-0.017,0.000701551994,0.0152284190645));
#12756=CARTESIAN_POINT('',(-0.0165,0.001,0.012961481397));
#12757=CARTESIAN_POINT('',(-0.0165,0.000801034662678128,0.0144727731752463));
#12758=CARTESIAN_POINT('',(-0.0165,0.000602069325356256,0.0159840649534926));
#12759=CARTESIAN_POINT('',(-0.0165,0.000403103988034383,0.0174953567317388));
#12760=CARTESIAN_POINT('',(-0.019981842228,0.,0.));
#12761=CARTESIAN_POINT('',(-0.0165,0.,0.));
#12762=CARTESIAN_POINT('',(-0.017,-0.000701551994,0.0152284190645));
#12763=CARTESIAN_POINT('',(-0.0165,-0.000403103988,0.017495356732));
#12764=CARTESIAN_POINT('',(-0.0165,-0.000602069325333334,0.0159840649536667));
#12765=CARTESIAN_POINT('',(-0.0165,-0.000801034662666668,0.0144727731753333));
#12766=CARTESIAN_POINT('',(-0.0165,-0.001,0.012961481397));
#12767=CARTESIAN_POINT('',(-0.017,-0.004038624693,0.014699878673));
#12768=CARTESIAN_POINT('',(-0.0165,-0.003054261508,0.012636118338));
#12769=CARTESIAN_POINT('',(-0.0165,-0.00371050363121451,0.0140119585610842));
#12770=CARTESIAN_POINT('',(-0.0165,-0.00436674575442903,0.0153877987841684));
#12771=CARTESIAN_POINT('',(-0.0165,-0.00502298787764354,0.0167636390072527));
#12772=CARTESIAN_POINT('',(-0.019981842228,0.,0.));
#12773=CARTESIAN_POINT('',(-0.0165,0.,0.));
#12774=CARTESIAN_POINT('',(-0.017,-0.005373055884,0.0142662956955));
#12775=CARTESIAN_POINT('',(-0.0165,-0.005789737228,0.016514507042));
#12776=CARTESIAN_POINT('',(-0.0165,-0.00551194966533333,0.0150156994776667));
#12777=CARTESIAN_POINT('',(-0.0165,-0.00523416210266667,0.0135168919133333));
#12778=CARTESIAN_POINT('',(-0.0165,-0.00495637454,0.012018084349));
#12779=CARTESIAN_POINT('',(-0.017,-0.008383472656,0.0127324117365));
#12780=CARTESIAN_POINT('',(-0.0165,-0.006809550619,0.011073843975));
#12781=CARTESIAN_POINT('',(-0.0165,-0.007858831977,0.012179555816));
#12782=CARTESIAN_POINT('',(-0.0165,-0.008908113335,0.013285267657));
#12783=CARTESIAN_POINT('',(-0.0165,-0.009957394693,0.014390979498));
#12784=CARTESIAN_POINT('',(-0.019981842228,0.,0.));
#12785=CARTESIAN_POINT('',(-0.0165,0.,0.));
#12786=CARTESIAN_POINT('',(-0.017,-0.00951860762750001,0.0119076879045));
#12787=CARTESIAN_POINT('',(-0.0165,-0.010609630648,0.013917102339));
#12788=CARTESIAN_POINT('',(-0.0165,-0.00988228196766668,0.012577492716));
#12789=CARTESIAN_POINT('',(-0.0165,-0.00915493328733334,0.011237883093));
#12790=CARTESIAN_POINT('',(-0.0165,-0.00842758460700001,0.00989827347));
#12791=CARTESIAN_POINT('',(-0.017,-0.0119076879045,0.00951860762750001));
#12792=CARTESIAN_POINT('',(-0.0165,-0.00989827347,0.00842758460700001));
#12793=CARTESIAN_POINT('',(-0.0165,-0.0112378830929259,0.00915493328729313));
#12794=CARTESIAN_POINT('',(-0.0165,-0.0125774927158519,0.00988228196758625));
#12795=CARTESIAN_POINT('',(-0.0165,-0.0139171023387778,0.0106096306478794));
#12796=CARTESIAN_POINT('',(-0.019981842228,0.,0.));
#12797=CARTESIAN_POINT('',(-0.0165,0.,0.));
#12798=CARTESIAN_POINT('',(-0.017,-0.0127324117365,0.008383472656));
#12799=CARTESIAN_POINT('',(-0.0165,-0.014390979498,0.009957394693));
#12800=CARTESIAN_POINT('',(-0.0165,-0.013285267657,0.008908113335));
#12801=CARTESIAN_POINT('',(-0.0165,-0.012179555816,0.007858831977));
#12802=CARTESIAN_POINT('',(-0.0165,-0.011073843975,0.006809550619));
#12803=CARTESIAN_POINT('',(-0.017,-0.0142662956955,0.005373055884));
#12804=CARTESIAN_POINT('',(-0.0165,-0.012018084349,0.00495637454));
#12805=CARTESIAN_POINT('',(-0.0165,-0.0135168919133333,0.00523416210266667));
#12806=CARTESIAN_POINT('',(-0.0165,-0.0150156994776667,0.00551194966533333));
#12807=CARTESIAN_POINT('',(-0.0165,-0.016514507042,0.005789737228));
#12808=CARTESIAN_POINT('',(-0.019981842228,0.,0.));
#12809=CARTESIAN_POINT('',(-0.0165,0.,0.));
#12810=CARTESIAN_POINT('',(-0.017,-0.014699878673,0.004038624693));
#12811=CARTESIAN_POINT('',(-0.0165,-0.016763639008,0.005022987878));
#12812=CARTESIAN_POINT('',(-0.0165,-0.0153877987846667,0.00436674575466666));
#12813=CARTESIAN_POINT('',(-0.0165,-0.0140119585613333,0.00371050363133333));
#12814=CARTESIAN_POINT('',(-0.0165,-0.012636118338,0.003054261508));
#12815=CARTESIAN_POINT('',(-0.017,-0.0152284190645,0.000701551994));
#12816=CARTESIAN_POINT('',(-0.0165,-0.012961481397,0.001));
#12817=CARTESIAN_POINT('',(-0.0165,-0.0144727731753372,0.000801034662666156));
#12818=CARTESIAN_POINT('',(-0.0165,-0.0159840649536667,0.000602069325333334));
#12819=CARTESIAN_POINT('',(-0.0165,-0.017495356732,0.000403103988));
#12820=CARTESIAN_POINT('',(-0.019981842228,0.,0.));
#12821=CARTESIAN_POINT('',(-0.0165,0.,0.));
#12822=CARTESIAN_POINT('',(-0.017,-0.0152284190645,-0.000701551994));
#12823=CARTESIAN_POINT('',(-0.0165,-0.0174953567319272,-0.000403103988009584));
#12824=CARTESIAN_POINT('',(-0.0165,-0.0159840649536181,-0.000602069325339723));
#12825=CARTESIAN_POINT('',(-0.0165,-0.0144727731753091,-0.000801034662669862));
#12826=CARTESIAN_POINT('',(-0.0165,-0.012961481397,-0.001));
#12827=CARTESIAN_POINT('',(-0.017,-0.014699878673,-0.004038624693));
#12828=CARTESIAN_POINT('',(-0.0165,-0.012636118338,-0.003054261508));
#12829=CARTESIAN_POINT('',(-0.0165,-0.0140119585612395,-0.00371050363128858));
#12830=CARTESIAN_POINT('',(-0.0165,-0.015387798784479,-0.00436674575457716));
#12831=CARTESIAN_POINT('',(-0.0165,-0.0167636390077185,-0.00502298787786573));
#12832=CARTESIAN_POINT('',(-0.019981842228,0.,0.));
#12833=CARTESIAN_POINT('',(-0.0165,0.,0.));
#12834=CARTESIAN_POINT('',(-0.017,-0.0142662956955,-0.005373055884));
#12835=CARTESIAN_POINT('',(-0.0165,-0.016514507042,-0.005789737228));
#12836=CARTESIAN_POINT('',(-0.0165,-0.0150156994776667,-0.00551194966533333));
#12837=CARTESIAN_POINT('',(-0.0165,-0.0135168919133333,-0.00523416210266667));
#12838=CARTESIAN_POINT('',(-0.0165,-0.012018084349,-0.00495637454));
#12839=CARTESIAN_POINT('',(-0.017,-0.0127324117365,-0.008383472656));
#12840=CARTESIAN_POINT('',(-0.0165,-0.011073843975,-0.006809550619));
#12841=CARTESIAN_POINT('',(-0.0165,-0.012179555815912,-0.00785883197691647));
#12842=CARTESIAN_POINT('',(-0.0165,-0.013285267656824,-0.00890811333483294));
#12843=CARTESIAN_POINT('',(-0.0165,-0.0143909794977359,-0.00995739469274941));
#12844=CARTESIAN_POINT('',(-0.019981842228,0.,0.));
#12845=CARTESIAN_POINT('',(-0.0165,0.,0.));
#12846=CARTESIAN_POINT('',(-0.017,-0.0119076879045,-0.00951860762750001));
#12847=CARTESIAN_POINT('',(-0.0165,-0.013917102339,-0.010609630648));
#12848=CARTESIAN_POINT('',(-0.0165,-0.012577492716,-0.00988228196766668));
#12849=CARTESIAN_POINT('',(-0.0165,-0.011237883093,-0.00915493328733334));
#12850=CARTESIAN_POINT('',(-0.0165,-0.00989827347,-0.00842758460700001));
#12851=CARTESIAN_POINT('',(-0.017,-0.00951860762750001,-0.0119076879045));
#12852=CARTESIAN_POINT('',(-0.0165,-0.00842758460700001,-0.00989827347));
#12853=CARTESIAN_POINT('',(-0.0165,-0.00915493328733334,-0.011237883093));
#12854=CARTESIAN_POINT('',(-0.0165,-0.00988228196766667,-0.012577492716));
#12855=CARTESIAN_POINT('',(-0.0165,-0.010609630648,-0.013917102339));
#12856=CARTESIAN_POINT('',(-0.019981842228,0.,0.));
#12857=CARTESIAN_POINT('',(-0.0165,0.,0.));
#12858=CARTESIAN_POINT('',(-0.017,-0.008383472656,-0.0127324117365));
#12859=CARTESIAN_POINT('',(-0.0165,-0.009957394693,-0.014390979498));
#12860=CARTESIAN_POINT('',(-0.0165,-0.008908113335,-0.013285267657));
#12861=CARTESIAN_POINT('',(-0.0165,-0.007858831977,-0.012179555816));
#12862=CARTESIAN_POINT('',(-0.0165,-0.006809550619,-0.011073843975));
#12863=CARTESIAN_POINT('',(-0.017,-0.005373055884,-0.0142662956955));
#12864=CARTESIAN_POINT('',(-0.0165,-0.00495637454,-0.012018084349));
#12865=CARTESIAN_POINT('',(-0.0165,-0.00523416210264554,-0.0135168919132194));
#12866=CARTESIAN_POINT('',(-0.0165,-0.00551194966529108,-0.0150156994774387));
#12867=CARTESIAN_POINT('',(-0.0165,-0.00578973722793662,-0.016514507041658));
#12868=CARTESIAN_POINT('',(-0.019981842228,0.,0.));
#12869=CARTESIAN_POINT('',(-0.0165,0.,0.));
#12870=CARTESIAN_POINT('',(-0.017,-0.004038624693,-0.014699878673));
#12871=CARTESIAN_POINT('',(-0.0165,-0.005022987878,-0.016763639008));
#12872=CARTESIAN_POINT('',(-0.0165,-0.00436674575466666,-0.0153877987846667));
#12873=CARTESIAN_POINT('',(-0.0165,-0.00371050363133333,-0.0140119585613333));
#12874=CARTESIAN_POINT('',(-0.0165,-0.003054261508,-0.012636118338));
#12875=CARTESIAN_POINT('',(-0.017,-0.000701551994,-0.0152284190645));
#12876=CARTESIAN_POINT('',(-0.0165,-0.001,-0.012961481397));
#12877=CARTESIAN_POINT('',(-0.0165,-0.000801034662666668,-0.0144727731753333));
#12878=CARTESIAN_POINT('',(-0.0165,-0.000602069325333334,-0.0159840649536667));
#12879=CARTESIAN_POINT('',(-0.0165,-0.000403103988,-0.017495356732));
#12880=CARTESIAN_POINT('',(-0.019981842228,0.,0.));
#12881=CARTESIAN_POINT('',(-0.0165,0.,0.));
#12882=CARTESIAN_POINT('',(-0.017,0.000701551994,-0.0152284190645));
#12883=CARTESIAN_POINT('',(-0.0165,0.000403103988,-0.017495356732));
#12884=CARTESIAN_POINT('',(-0.0165,0.000602069325333334,-0.0159840649536667));
#12885=CARTESIAN_POINT('',(-0.0165,0.000801034662666668,-0.0144727731753333));
#12886=CARTESIAN_POINT('',(-0.0165,0.001,-0.012961481397));
#12887=CARTESIAN_POINT('',(-0.017,0.004038624693,-0.014699878673));
#12888=CARTESIAN_POINT('',(-0.0165,0.003054261508,-0.012636118338));
#12889=CARTESIAN_POINT('',(-0.0165,0.00371050363132807,-0.0140119585613223));
#12890=CARTESIAN_POINT('',(-0.0165,0.00436674575466666,-0.0153877987846667));
#12891=CARTESIAN_POINT('',(-0.0165,0.005022987878,-0.016763639008));
#12892=CARTESIAN_POINT('',(-0.019981842228,0.,0.));
#12893=CARTESIAN_POINT('',(-0.0165,0.,0.));
#12894=CARTESIAN_POINT('',(-0.017,0.005373055884,-0.0142662956955));
#12895=CARTESIAN_POINT('',(-0.0165,0.005789737228,-0.016514507042));
#12896=CARTESIAN_POINT('',(-0.0165,0.00551194966533333,-0.0150156994776667));
#12897=CARTESIAN_POINT('',(-0.0165,0.00523416210266667,-0.0135168919133333));
#12898=CARTESIAN_POINT('',(-0.0165,0.00495637454,-0.012018084349));
#12899=CARTESIAN_POINT('',(-0.017,0.008383472656,-0.0127324117365));
#12900=CARTESIAN_POINT('',(-0.0165,0.006809550619,-0.011073843975));
#12901=CARTESIAN_POINT('',(-0.0165,0.00785883197697961,-0.0121795558159785));
#12902=CARTESIAN_POINT('',(-0.0165,0.00890811333495922,-0.013285267656957));
#12903=CARTESIAN_POINT('',(-0.0165,0.00995739469293883,-0.0143909794979355));
#12904=CARTESIAN_POINT('',(-0.019981842228,0.,0.));
#12905=CARTESIAN_POINT('',(-0.0165,0.,0.));
#12906=CARTESIAN_POINT('',(-0.017,0.00951860762750001,-0.0119076879045));
#12907=CARTESIAN_POINT('',(-0.0165,0.010609630648,-0.013917102339));
#12908=CARTESIAN_POINT('',(-0.0165,0.00988228196766668,-0.012577492716));
#12909=CARTESIAN_POINT('',(-0.0165,0.00915493328733334,-0.011237883093));
#12910=CARTESIAN_POINT('',(-0.0165,0.00842758460700001,-0.00989827347));
#12911=CARTESIAN_POINT('',(-0.017,0.0119076879045,-0.00951860762750001));
#12912=CARTESIAN_POINT('',(-0.0165,0.00989827347,-0.00842758460700001));
#12913=CARTESIAN_POINT('',(-0.0165,0.011237883093,-0.00915493328733334));
#12914=CARTESIAN_POINT('',(-0.0165,0.012577492716,-0.00988228196766667));
#12915=CARTESIAN_POINT('',(-0.0165,0.013917102339,-0.010609630648));
#12916=CARTESIAN_POINT('',(-0.019981842228,0.,0.));
#12917=CARTESIAN_POINT('',(-0.0165,0.,0.));
#12918=CARTESIAN_POINT('',(-0.017,0.0127324117365,-0.008383472656));
#12919=CARTESIAN_POINT('',(-0.0165,0.014390979498,-0.009957394693));
#12920=CARTESIAN_POINT('',(-0.0165,0.013285267657,-0.008908113335));
#12921=CARTESIAN_POINT('',(-0.0165,0.012179555816,-0.007858831977));
#12922=CARTESIAN_POINT('',(-0.0165,0.011073843975,-0.006809550619));
#12923=CARTESIAN_POINT('',(-0.017,0.0142662956955,-0.005373055884));
#12924=CARTESIAN_POINT('',(-0.0165,0.012018084349,-0.00495637454));
#12925=CARTESIAN_POINT('',(-0.0165,0.0135168919133095,-0.00523416210266226));
#12926=CARTESIAN_POINT('',(-0.0165,0.0150156994776191,-0.00551194966532451));
#12927=CARTESIAN_POINT('',(-0.0165,0.0165145070419286,-0.00578973722798677));
#12928=CARTESIAN_POINT('',(-0.019981842228,0.,0.));
#12929=CARTESIAN_POINT('',(-0.0165,0.,0.));
#12930=CARTESIAN_POINT('',(-0.017,0.014699878673,-0.004038624693));
#12931=CARTESIAN_POINT('',(-0.0165,0.016763639008,-0.005022987878));
#12932=CARTESIAN_POINT('',(-0.0165,0.0153877987846667,-0.00436674575466666));
#12933=CARTESIAN_POINT('',(-0.0165,0.0140119585613333,-0.00371050363133333));
#12934=CARTESIAN_POINT('',(-0.0165,0.012636118338,-0.003054261508));
#12935=CARTESIAN_POINT('',(-0.017,0.0152284190645,-0.000701551994));
#12936=CARTESIAN_POINT('',(-0.0165,0.012961481397,-0.001));
#12937=CARTESIAN_POINT('',(-0.0165,0.0144727731751553,-0.000801034662690101));
#12938=CARTESIAN_POINT('',(-0.0165,0.0159840649533107,-0.000602069325380202));
#12939=CARTESIAN_POINT('',(-0.0165,0.017495356731466,-0.000403103988070302));
#12940=CARTESIAN_POINT('',(-0.034017463007,0.,0.));
#12941=CARTESIAN_POINT('',(-0.021,0.,0.));
#12942=CARTESIAN_POINT('',(-0.021,0.,0.0175));
#12943=CARTESIAN_POINT('',(-0.0165,0.0152307406985,-2.60208521396521E-20));
#12944=CARTESIAN_POINT('',(-0.0165,0.0143908616785,0.0044219993675));
#12945=CARTESIAN_POINT('',(-0.018,0.,-3.07046055247895E-18));
#12946=CARTESIAN_POINT('',(-0.018,0.,0.));
#12947=CARTESIAN_POINT('',(-0.018,0.,0.0165));
#12948=CARTESIAN_POINT('',(-0.0165,-0.0152307406985,-2.60208521396521E-20));
#12949=CARTESIAN_POINT('',(-0.0165,-0.0143908616785,0.0044219993675));
#12950=CARTESIAN_POINT('',(-0.0165,-0.012144626484,0.00870959063300001));
#12951=CARTESIAN_POINT('',(-0.0165,-0.00870959063300002,0.012144626484));
#12952=CARTESIAN_POINT('',(-0.0165,-0.0044219993675,0.0143908616785));
#12953=CARTESIAN_POINT('',(-0.0165,-1.74556549770166E-19,0.0152330629486464));
#12954=CARTESIAN_POINT('',(-0.0165,0.0044219993675,0.0143908616785));
#12955=CARTESIAN_POINT('',(-0.0165,0.00870959063300002,0.012144626484));
#12956=CARTESIAN_POINT('',(-0.0165,0.012144626484,0.00870959063300001));
#12957=CARTESIAN_POINT('',(-0.0165,0.0143908616785,-0.0044219993675));
#12958=CARTESIAN_POINT('',(-0.0165,0.012144626484,-0.00870959063300003));
#12959=CARTESIAN_POINT('',(-0.0165,0.00870959063300002,-0.012144626484));
#12960=CARTESIAN_POINT('',(-0.0165,0.0044219993675,-0.0143908616785));
#12961=CARTESIAN_POINT('',(-0.0165,-1.74556549770166E-19,-0.0152330629486464));
#12962=CARTESIAN_POINT('',(-0.0165,-0.0044219993675,-0.0143908616785));
#12963=CARTESIAN_POINT('',(-0.0165,-0.00870959063300002,-0.012144626484));
#12964=CARTESIAN_POINT('',(-0.0165,-0.012144626484,-0.00870959063300003));
#12965=CARTESIAN_POINT('',(-0.0165,-0.0143908616785,-0.0044219993675));
#12966=CARTESIAN_POINT('',(-0.021,0.,-3.07046055247895E-18));
#12967=CARTESIAN_POINT('',(-0.021,0.,0.));
#12968=CARTESIAN_POINT('',(-0.021,0.,0.0165));
#12969=CARTESIAN_POINT('',(-0.034017463007,0.,0.));
#12970=CARTESIAN_POINT('',(0.0175000000000004,0.046,1.10617214860196E-34));
#12971=CARTESIAN_POINT('',(-0.00525,0.,0.));
#12972=CARTESIAN_POINT('',(0.00525,0.,0.));
#12973=CARTESIAN_POINT('',(0.00525,0.,-0.0075));
#12974=CARTESIAN_POINT('',(-0.00525,0.,0.));
#12975=CARTESIAN_POINT('',(-0.00525,0.,-0.0075));
#12976=CARTESIAN_POINT('',(0.00525,-4.9439619065339E-19,-2.41993924898764E-18));
#12977=CARTESIAN_POINT('',(0.00525000000022048,1.9259841093292E-13,4.25226277214903E-19));
#12978=CARTESIAN_POINT('',(0.00525000000023268,0.00800000000074963,4.25226277214903E-19));
#12979=CARTESIAN_POINT('',(-0.00525,-5.50774703622636E-19,-8.67361737988404E-21));
#12980=CARTESIAN_POINT('',(-0.00525000000022048,1.92852798037857E-13,-1.01440902624871E-18));
#12981=CARTESIAN_POINT('',(-0.00525000000023269,0.0120000000007499,-1.01440902624871E-18));
#12982=CARTESIAN_POINT('',(0.00474999999987469,1.93361039494021E-13,4.45859022211667E-19));
#12983=CARTESIAN_POINT('',(0.00475000000055703,-1.93360444885966E-13,-1.48019874151438E-19));
#12984=CARTESIAN_POINT('',(0.00474999987540352,-1.74337662513279E-12,-0.00850000000012328));
#12985=CARTESIAN_POINT('',(0.00474999987527852,-4.86361310422452E-12,0.00850000000012328));
#12986=CARTESIAN_POINT('',(0.00475000000055704,-4.86361227985766E-12,0.00850000000024656));
#12987=CARTESIAN_POINT('',(0.00475000000055534,-0.00111264740275087,0.0084999999995846));
#12988=CARTESIAN_POINT('',(0.00475000000055195,-0.00333742350645399,0.00805742090693034));
#12989=CARTESIAN_POINT('',(0.00475000000054763,-0.00616690169649648,0.00616688297620523));
#12990=CARTESIAN_POINT('',(0.00475000000054475,-0.00805741556199689,0.00333749301577175));
#12991=CARTESIAN_POINT('',(0.00475000000054374,-0.00872129221938764,-1.60072261902693E-12));
#12992=CARTESIAN_POINT('',(0.00475000000054475,-0.00805741556077174,-0.00333749301872954));
#12993=CARTESIAN_POINT('',(0.00475000000054763,-0.00616690169423269,-0.00616688297846902));
#12994=CARTESIAN_POINT('',(0.00475000000055195,-0.00333742350349621,-0.00805742090815546));
#12995=CARTESIAN_POINT('',(0.00475000000055534,-0.00111264739963064,-0.00849999999999304));
#12996=CARTESIAN_POINT('',(0.00475000000055704,-1.7433859526852E-12,-0.00850000000024656));
#12997=CARTESIAN_POINT('',(-0.00474999999987469,1.93361391425766E-13,-1.00192510578618E-18));
#12998=CARTESIAN_POINT('',(-0.00424999999977952,1.92851057078383E-13,-6.6309546838198E-19));
#12999=CARTESIAN_POINT('',(-0.00424999999976732,0.0120000000007499,-6.6309546838198E-19));
#13000=CARTESIAN_POINT('',(-0.007263258046,0.,2.86039083864497E-51));
#13001=CARTESIAN_POINT('',(0.00425,-5.61175846058392E-12,-0.0085));
#13002=CARTESIAN_POINT('',(0.00425,-0.00111264740337218,-0.00849999999926542));
#13003=CARTESIAN_POINT('',(0.00425,-0.00333742350679297,-0.00805742090655498));
#13004=CARTESIAN_POINT('',(0.00425,-0.00616690169647487,-0.00616688297600855));
#13005=CARTESIAN_POINT('',(0.00425,-0.008057415561805,-0.00333749301594122));
#13006=CARTESIAN_POINT('',(0.00425,-0.00872129221928992,1.00565516758058E-12));
#13007=CARTESIAN_POINT('',(0.00425,-0.00805741556103531,0.00333749301779943));
#13008=CARTESIAN_POINT('',(0.00425,-0.00616690169505265,0.00616688297743077));
#13009=CARTESIAN_POINT('',(0.00425,-0.00333742350493477,0.00805742090732466));
#13010=CARTESIAN_POINT('',(0.00425,-0.0011126474014119,0.00849999999952203));
#13011=CARTESIAN_POINT('',(0.00425,-3.65148430959518E-12,0.0085));
#13012=CARTESIAN_POINT('',(0.00425,-2.88824233062088E-12,0.0085));
#13013=CARTESIAN_POINT('',(0.00425000037472148,-1.74337673725018E-12,-0.00850000000012328));
#13014=CARTESIAN_POINT('',(0.00425,0.,1.20303851022306E-18));
#13015=CARTESIAN_POINT('',(0.00425000000012531,1.93360815258866E-13,-2.80147189803738E-19));
#13016=CARTESIAN_POINT('',(0.00374999999977953,-2.71834574313571E-12,0.00800000000055703));
#13017=CARTESIAN_POINT('',(0.00374999999978272,-0.00209439510486201,0.00799999999979495));
#13018=CARTESIAN_POINT('',(0.00374999999978908,-0.00626651094914304,0.00626889299797267));
#13019=CARTESIAN_POINT('',(0.00374999999979305,-0.00886674452618622,-5.97131919231566E-13));
#13020=CARTESIAN_POINT('',(0.00374999999978908,-0.00626651094829869,-0.00626889299881671));
#13021=CARTESIAN_POINT('',(0.00374999999978272,-0.00209439510378449,-0.00800000000007704));
#13022=CARTESIAN_POINT('',(0.00374999999977953,-1.64082385457008E-12,-0.00800000000055703));
#13023=CARTESIAN_POINT('',(0.00374999987488976,-2.71834529339123E-12,0.00800000000027852));
#13024=CARTESIAN_POINT('',(0.00374999987488976,-1.64082717271973E-12,-0.00800000000040351));
#13025=CARTESIAN_POINT('',(0.00374999999977952,-1.92598860655761E-13,1.48862633905608E-19));
#13026=CARTESIAN_POINT('',(-0.00425,-5.50774703622636E-19,8.67361737988404E-21));
#13027=CARTESIAN_POINT('',(-0.00425000000022048,1.94006876112138E-13,-2.13954723767001E-19));
#13028=CARTESIAN_POINT('',(-0.00425000000020828,0.00949999999963698,-2.13954723767001E-19));
#13029=CARTESIAN_POINT('',(-0.007263258046,0.,2.83936039877452E-51));
#13030=CARTESIAN_POINT('',(0.001457106781,-5.28165502172604E-12,-0.008));
#13031=CARTESIAN_POINT('',(0.001457106781,-0.00209439510694832,-0.00799999999861726));
#13032=CARTESIAN_POINT('',(0.001457106781,-0.00626651094977711,-0.00626889299625425));
#13033=CARTESIAN_POINT('',(0.001457106781,-0.00886674452547288,1.0224280356647E-12));
#13034=CARTESIAN_POINT('',(0.001457106781,-0.00626651094833137,0.00626889299769943));
#13035=CARTESIAN_POINT('',(0.001457106781,-0.00209439510510336,0.00799999999910028));
#13036=CARTESIAN_POINT('',(0.001457106781,-3.43669111491311E-12,0.008));
#13037=CARTESIAN_POINT('',(0.001457106781,-2.7183457229373E-12,0.008));
#13038=CARTESIAN_POINT('',(0.001457107156,-2.28165122079125E-12,-0.008));
#13039=CARTESIAN_POINT('',(0.001457106781,0.,9.68154981406677E-19));
#13040=CARTESIAN_POINT('',(-0.00374999999987468,1.93364582630688E-13,-2.28558934437229E-19));
#13041=CARTESIAN_POINT('',(-0.00375,0.,0.));
#13042=CARTESIAN_POINT('',(-0.00374999987527851,-1.8459280570297E-12,-0.00899999999987672));
#13043=CARTESIAN_POINT('',(-0.00374999987527851,-1.22168301791654E-12,0.00899999999987672));
#13044=CARTESIAN_POINT('',(-0.00375000000055703,-1.22168309480298E-12,0.00899999999975343));
#13045=CARTESIAN_POINT('',(-0.00375000000055552,-0.00117809724617388,0.00899999999961883));
#13046=CARTESIAN_POINT('',(-0.00375000000055249,-0.00353374253293338,0.00853138684369092));
#13047=CARTESIAN_POINT('',(-0.00375000000054865,-0.0065296606176239,0.00652964080030454));
#13048=CARTESIAN_POINT('',(-0.00375000000054607,-0.00853138118227796,0.00353381613659912));
#13049=CARTESIAN_POINT('',(-0.00375000000054517,-0.00923430940871994,3.20239732450106E-13));
#13050=CARTESIAN_POINT('',(-0.00375000000054607,-0.00853138118252307,-0.00353381613600736));
#13051=CARTESIAN_POINT('',(-0.00375000000054865,-0.0065296606180768,-0.00652964079985164));
#13052=CARTESIAN_POINT('',(-0.00375000000055249,-0.00353374253352514,-0.00853138684344582));
#13053=CARTESIAN_POINT('',(-0.00375000000055552,-0.00117809724679812,-0.00899999999953711));
#13054=CARTESIAN_POINT('',(-0.00375000000055703,-1.845925958314E-12,-0.00899999999975343));
#13055=CARTESIAN_POINT('',(0.0014571067816285,-5.47396505703968E-13,6.65202876568241E-20));
#13056=CARTESIAN_POINT('',(0.00110355339071671,1.58556738773517E-17,0.00814644660952611));
#13057=CARTESIAN_POINT('',(0.00119611345182742,2.63259265651322E-16,0.00805388654805348));
#13058=CARTESIAN_POINT('',(0.00132620708739174,-1.64577341757993E-15,0.00799999999964119));
#13059=CARTESIAN_POINT('',(0.0014571067814045,1.67659206997871E-17,0.00799999999958255));
#13060=CARTESIAN_POINT('',(0.00110355330247001,-2.9115133713822E-12,0.0081464466976514));
#13061=CARTESIAN_POINT('',(0.00110355339071671,-1.6708634304086E-12,-0.00814644660952611));
#13062=CARTESIAN_POINT('',(0.00110355339048919,-0.00213273473648634,-0.00814644660922211));
#13063=CARTESIAN_POINT('',(0.00110355339003597,-0.0063812246085619,-0.0063836502643864));
#13064=CARTESIAN_POINT('',(0.00110355338975351,-0.00902905761052969,-6.87539018106074E-13));
#13065=CARTESIAN_POINT('',(0.00110355339003597,-0.00638122460953407,0.00638365026341459));
#13066=CARTESIAN_POINT('',(0.00110355339048919,-0.00213273473772698,0.00814644660889731));
#13067=CARTESIAN_POINT('',(0.00110355339071671,-2.91151058367133E-12,0.00814644660952611));
#13068=CARTESIAN_POINT('',(0.00110355330262237,-1.67086175802321E-12,-0.00814644669762802));
#13069=CARTESIAN_POINT('',(0.0014571067814045,-3.13787920007409E-17,-0.00799999999958255));
#13070=CARTESIAN_POINT('',(0.00132620708739174,-1.66845701558407E-15,-0.00799999999964119));
#13071=CARTESIAN_POINT('',(0.00119611345182742,2.65760905900004E-16,-0.00805388654805348));
#13072=CARTESIAN_POINT('',(0.00110355339071671,4.46112367465754E-17,-0.00814644660952611));
#13073=CARTESIAN_POINT('',(0.0014571067816285,5.47397208070073E-13,-5.45798719985721E-19));
#13074=CARTESIAN_POINT('',(0.00110355339112794,0.,-1.04204690494148E-15));
#13075=CARTESIAN_POINT('',(-0.007263258046,0.,0.));
#13076=CARTESIAN_POINT('',(-0.003116025404,-3.86627750427725E-12,0.009));
#13077=CARTESIAN_POINT('',(-0.003116025404,-0.00117809724855378,0.0089999999994939));
#13078=CARTESIAN_POINT('',(-0.003116025404,-0.00353374253463681,0.00853138684304964));
#13079=CARTESIAN_POINT('',(-0.003116025404,-0.00652966061829104,0.00652964079963258));
#13080=CARTESIAN_POINT('',(-0.003116025404,-0.00853138118227268,0.00353381613649351));
#13081=CARTESIAN_POINT('',(-0.003116025404,-0.00923430940865992,1.06481072844012E-12));
#13082=CARTESIAN_POINT('',(-0.003116025404,-0.00853138118308765,-0.003533816134526));
#13083=CARTESIAN_POINT('',(-0.003116025404,-0.00652966061979692,-0.0065296407981267));
#13084=CARTESIAN_POINT('',(-0.003116025404,-0.00353374253660432,-0.00853138684223469));
#13085=CARTESIAN_POINT('',(-0.003116025404,-0.00117809725062936,-0.00899999999922221));
#13086=CARTESIAN_POINT('',(-0.003116025404,-5.9418618994418E-12,-0.009));
#13087=CARTESIAN_POINT('',(-0.00311602552873704,-1.84592937600593E-12,-0.00899999999997601));
#13088=CARTESIAN_POINT('',(-0.00311602552873704,1.12499936185184E-12,0.00899999999997601));
#13089=CARTESIAN_POINT('',(-0.003116025404,0.,0.));
#13090=CARTESIAN_POINT('',(0.00925000000025689,0.,-1.03355916846639E-15));
#13091=CARTESIAN_POINT('',(0.000896446609127943,0.,-1.04226268832191E-15));
#13092=CARTESIAN_POINT('',(0.000896446947516299,-2.38248677279272E-12,-0.00835355305274167));
#13093=CARTESIAN_POINT('',(0.000896446609127934,-2.83848445413882E-12,0.00835355339112793));
#13094=CARTESIAN_POINT('',(0.000896446609127957,-5.51507340218912E-12,-0.00835355339113002));
#13095=CARTESIAN_POINT('',(0.000896446609127957,-0.00109347758700829,-0.0083535533904081));
#13096=CARTESIAN_POINT('',(0.000896446609127956,-0.00327992299444752,-0.00791859949855468));
#13097=CARTESIAN_POINT('',(0.000896446609127955,-0.00606065206815843,-0.00606063367022831));
#13098=CARTESIAN_POINT('',(0.000896446609127951,-0.00791859424588842,-0.00327999130602281));
#13099=CARTESIAN_POINT('',(0.000896446609127948,-0.00857103296393836,9.87285581686735E-13));
#13100=CARTESIAN_POINT('',(0.000896446609127945,-0.00791859424513199,0.00327999130784692));
#13101=CARTESIAN_POINT('',(0.000896446609127942,-0.00606065206676072,0.00606063367162394));
#13102=CARTESIAN_POINT('',(0.00089644660912794,-0.00327992299262134,0.00791859949930901));
#13103=CARTESIAN_POINT('',(0.000896446609127939,-0.00109347758508179,0.00835355339065819));
#13104=CARTESIAN_POINT('',(0.000896446609127939,-3.58857283965566E-12,0.00835355339112793));
#13105=CARTESIAN_POINT('',(-0.00311602540366083,1.89369138590977E-13,4.60164670987285E-19));
#13106=CARTESIAN_POINT('',(-0.00311602540347409,-2.08135904343245E-17,0.00899999999995202));
#13107=CARTESIAN_POINT('',(-0.00276695955312565,-2.17671273402248E-15,0.00899999999988684));
#13108=CARTESIAN_POINT('',(-0.00242453292500672,-2.5821733949979E-16,0.00880229989405671));
#13109=CARTESIAN_POINT('',(-0.00224999999965417,-1.04806440198648E-18,0.0085000000001643));
#13110=CARTESIAN_POINT('',(-0.00224999987482708,-1.83738466424475E-19,0.00850000000008215));
#13111=CARTESIAN_POINT('',(-0.00224999999965417,2.2030464917804E-13,4.66825340357479E-19));
#13112=CARTESIAN_POINT('',(-0.00224999987482708,-1.74337942337899E-12,-0.00850000000008215));
#13113=CARTESIAN_POINT('',(-0.00224999999965417,-1.44542388119606E-17,-0.0085000000001643));
#13114=CARTESIAN_POINT('',(-0.00242453292500672,-2.56372140876474E-16,-0.00880229989405671));
#13115=CARTESIAN_POINT('',(-0.00276695955312565,-2.15760081618848E-15,-0.00899999999988684));
#13116=CARTESIAN_POINT('',(-0.00311602540347409,1.49516727692217E-17,-0.00899999999995202));
#13117=CARTESIAN_POINT('',(-0.00311602540366083,-1.89369495587902E-13,-4.56753702428283E-19));
#13118=CARTESIAN_POINT('',(-0.00224999999965417,-1.74337645012797E-12,-0.0085000000001643));
#13119=CARTESIAN_POINT('',(-0.00224999999969392,-0.00111264739985699,-0.00849999999996493));
#13120=CARTESIAN_POINT('',(-0.00224999999977339,-0.00333742350419627,-0.00805742090804886));
#13121=CARTESIAN_POINT('',(-0.00224999999987446,-0.00616690169538636,-0.00616688297774479));
#13122=CARTESIAN_POINT('',(-0.002249999999942,-0.00805741556187121,-0.00333749301710294));
#13123=CARTESIAN_POINT('',(-0.00224999999996571,-0.00872129221981244,8.94381676439934E-13));
#13124=CARTESIAN_POINT('',(-0.002249999999942,-0.00805741556118667,0.00333749301875555));
#13125=CARTESIAN_POINT('',(-0.00224999999987446,-0.00616690169412152,0.00616688297900963));
#13126=CARTESIAN_POINT('',(-0.00224999999977339,-0.00333742350254365,0.00805742090873338));
#13127=CARTESIAN_POINT('',(-0.00224999999969392,-0.00111264739811362,0.00850000000019314));
#13128=CARTESIAN_POINT('',(-0.00224999999965417,-1.35791309261817E-17,0.0085000000001643));
#13129=CARTESIAN_POINT('',(0.000542893218371495,5.47403523416524E-13,1.10783975326665E-19));
#13130=CARTESIAN_POINT('',(0.000896446609283292,-1.46288588890009E-17,0.0083535533904739));
#13131=CARTESIAN_POINT('',(0.000803886548172581,-5.03456191566966E-16,0.00844611345194653));
#13132=CARTESIAN_POINT('',(0.00067379291260826,-1.94773245151004E-15,0.00850000000035882));
#13133=CARTESIAN_POINT('',(0.000542893218595496,1.69082711704543E-17,0.00850000000041746));
#13134=CARTESIAN_POINT('',(0.000542893093797748,-2.12500021499821E-12,0.00850000000020873));
#13135=CARTESIAN_POINT('',(0.000542893218595496,-2.12499836668962E-12,0.00850000000041746));
#13136=CARTESIAN_POINT('',(0.000542893218721609,-0.00111264740011923,0.00850000000006764));
#13137=CARTESIAN_POINT('',(0.000542893218973776,-0.00333742350416026,0.00805742090796045));
#13138=CARTESIAN_POINT('',(0.000542893219294483,-0.00616690169492879,0.00616688297771508));
#13139=CARTESIAN_POINT('',(0.000542893219508763,-0.00805741556119902,0.00333749301739052));
#13140=CARTESIAN_POINT('',(0.00054289321958401,-0.00872129221924304,-1.95784323807277E-13));
#13141=CARTESIAN_POINT('',(0.000542893219508763,-0.00805741556104918,-0.00333749301775226));
#13142=CARTESIAN_POINT('',(0.000542893219294483,-0.00616690169465192,-0.00616688297799194));
#13143=CARTESIAN_POINT('',(0.000542893218973777,-0.00333742350379851,-0.00805742090811029));
#13144=CARTESIAN_POINT('',(0.000542893218721609,-0.00111264739973761,-0.0085000000001176));
#13145=CARTESIAN_POINT('',(0.000542893218595496,-1.74337804822321E-12,-0.00850000000041746));
#13146=CARTESIAN_POINT('',(0.000542893093922748,-1.7433764476282E-12,-0.00850000000020873));
#13147=CARTESIAN_POINT('',(0.000542893218595496,1.61471761803093E-18,-0.00850000000041746));
#13148=CARTESIAN_POINT('',(0.000673792912608261,-1.96176775230103E-15,-0.00850000000035882));
#13149=CARTESIAN_POINT('',(0.000803886548172583,-5.16138536658815E-16,-0.00844611345194653));
#13150=CARTESIAN_POINT('',(0.000896446609283294,-2.59491966845735E-17,-0.0083535533904739));
#13151=CARTESIAN_POINT('',(0.000542893218371494,-5.47404119942789E-13,5.87721542220263E-20));
#13152=CARTESIAN_POINT('',(0.000542893218595497,-5.47404119968178E-13,5.87721541987024E-20));
#13153=CARTESIAN_POINT('',(-0.007263258046,0.,2.44324620272917E-53));
#13154=CARTESIAN_POINT('',(0.0175000000000005,-0.06775,1.10617214860196E-34));
#13155=CARTESIAN_POINT('',(-0.00525,0.,0.));
#13156=CARTESIAN_POINT('',(0.00525,0.,0.));
#13157=CARTESIAN_POINT('',(0.00525,0.,-0.0075));
#13158=CARTESIAN_POINT('',(-0.00525,0.,0.));
#13159=CARTESIAN_POINT('',(-0.00525,0.,-0.0075));
#13160=CARTESIAN_POINT('',(0.00525,-4.9439619065339E-19,-2.41993924898764E-18));
#13161=CARTESIAN_POINT('',(0.00525000000022048,1.9259841093292E-13,4.25226277214903E-19));
#13162=CARTESIAN_POINT('',(0.00525000000023268,0.00800000000074963,4.25226277214903E-19));
#13163=CARTESIAN_POINT('',(-0.00525,-2.64545330086463E-19,6.93889390390723E-19));
#13164=CARTESIAN_POINT('',(-0.00525000000022048,1.92806907086136E-13,-4.70350263194859E-19));
#13165=CARTESIAN_POINT('',(-0.00525000000023268,0.0110000000007498,-4.70350263194859E-19));
#13166=CARTESIAN_POINT('',(0.00474999999987469,1.93361039494021E-13,4.45859022211667E-19));
#13167=CARTESIAN_POINT('',(0.00475000000055703,-1.93360444885966E-13,-1.48019874151438E-19));
#13168=CARTESIAN_POINT('',(0.00474999987540352,-1.74337662513279E-12,-0.00850000000012328));
#13169=CARTESIAN_POINT('',(0.00474999987527852,-4.86361310422452E-12,0.00850000000012328));
#13170=CARTESIAN_POINT('',(0.00475000000055704,-4.86361227985766E-12,0.00850000000024656));
#13171=CARTESIAN_POINT('',(0.00475000000055534,-0.00111264740275087,0.0084999999995846));
#13172=CARTESIAN_POINT('',(0.00475000000055195,-0.00333742350645399,0.00805742090693034));
#13173=CARTESIAN_POINT('',(0.00475000000054763,-0.00616690169649648,0.00616688297620523));
#13174=CARTESIAN_POINT('',(0.00475000000054475,-0.00805741556199689,0.00333749301577175));
#13175=CARTESIAN_POINT('',(0.00475000000054374,-0.00872129221938764,-1.60072261902693E-12));
#13176=CARTESIAN_POINT('',(0.00475000000054475,-0.00805741556077174,-0.00333749301872954));
#13177=CARTESIAN_POINT('',(0.00475000000054763,-0.00616690169423269,-0.00616688297846902));
#13178=CARTESIAN_POINT('',(0.00475000000055195,-0.00333742350349621,-0.00805742090815546));
#13179=CARTESIAN_POINT('',(0.00475000000055534,-0.00111264739963064,-0.00849999999999304));
#13180=CARTESIAN_POINT('',(0.00475000000055704,-1.7433859526852E-12,-0.00850000000024656));
#13181=CARTESIAN_POINT('',(-0.00474999999987469,1.93361681362568E-13,-4.6302299312396E-19));
#13182=CARTESIAN_POINT('',(-0.00424999999977952,1.92803729271711E-13,2.29417486392181E-19));
#13183=CARTESIAN_POINT('',(-0.00424999999976731,0.0110000000007498,2.29417486392181E-19));
#13184=CARTESIAN_POINT('',(-0.007263258046,0.,2.86039083864497E-51));
#13185=CARTESIAN_POINT('',(0.00425,-5.61175846058392E-12,-0.0085));
#13186=CARTESIAN_POINT('',(0.00425,-0.00111264740337218,-0.00849999999926542));
#13187=CARTESIAN_POINT('',(0.00425,-0.00333742350679297,-0.00805742090655498));
#13188=CARTESIAN_POINT('',(0.00425,-0.00616690169647487,-0.00616688297600855));
#13189=CARTESIAN_POINT('',(0.00425,-0.008057415561805,-0.00333749301594122));
#13190=CARTESIAN_POINT('',(0.00425,-0.00872129221928992,1.00565516758058E-12));
#13191=CARTESIAN_POINT('',(0.00425,-0.00805741556103531,0.00333749301779943));
#13192=CARTESIAN_POINT('',(0.00425,-0.00616690169505265,0.00616688297743077));
#13193=CARTESIAN_POINT('',(0.00425,-0.00333742350493477,0.00805742090732466));
#13194=CARTESIAN_POINT('',(0.00425,-0.0011126474014119,0.00849999999952203));
#13195=CARTESIAN_POINT('',(0.00425,-3.65148430959518E-12,0.0085));
#13196=CARTESIAN_POINT('',(0.00425,-2.88824233062088E-12,0.0085));
#13197=CARTESIAN_POINT('',(0.00425000037472148,-1.74337673725018E-12,-0.00850000000012328));
#13198=CARTESIAN_POINT('',(0.00425,0.,1.20303851022306E-18));
#13199=CARTESIAN_POINT('',(0.00425000000012531,1.93360815258866E-13,-2.80147189803738E-19));
#13200=CARTESIAN_POINT('',(0.00374999999977953,-2.71834574313571E-12,0.00800000000055703));
#13201=CARTESIAN_POINT('',(0.00374999999978272,-0.00209439510486201,0.00799999999979495));
#13202=CARTESIAN_POINT('',(0.00374999999978908,-0.00626651094914304,0.00626889299797267));
#13203=CARTESIAN_POINT('',(0.00374999999979305,-0.00886674452618622,-5.97131919231566E-13));
#13204=CARTESIAN_POINT('',(0.00374999999978908,-0.00626651094829869,-0.00626889299881671));
#13205=CARTESIAN_POINT('',(0.00374999999978272,-0.00209439510378449,-0.00800000000007704));
#13206=CARTESIAN_POINT('',(0.00374999999977953,-1.64082385457008E-12,-0.00800000000055703));
#13207=CARTESIAN_POINT('',(0.00374999987488976,-2.71834529339123E-12,0.00800000000027852));
#13208=CARTESIAN_POINT('',(0.00374999987488976,-1.64082717271973E-12,-0.00800000000040351));
#13209=CARTESIAN_POINT('',(0.00374999999977952,-1.92598860655761E-13,1.48862633905608E-19));
#13210=CARTESIAN_POINT('',(-0.00425,-2.64545330086463E-19,-6.93889390390723E-19));
#13211=CARTESIAN_POINT('',(-0.00425000000022048,1.94006876112138E-13,-2.13954723767001E-19));
#13212=CARTESIAN_POINT('',(-0.00425000000020828,0.00949999999963698,-2.13954723767001E-19));
#13213=CARTESIAN_POINT('',(-0.007263258046,0.,2.83936039877452E-51));
#13214=CARTESIAN_POINT('',(0.001457106781,-5.28165502172604E-12,-0.008));
#13215=CARTESIAN_POINT('',(0.001457106781,-0.00209439510694832,-0.00799999999861726));
#13216=CARTESIAN_POINT('',(0.001457106781,-0.00626651094977711,-0.00626889299625425));
#13217=CARTESIAN_POINT('',(0.001457106781,-0.00886674452547288,1.0224280356647E-12));
#13218=CARTESIAN_POINT('',(0.001457106781,-0.00626651094833137,0.00626889299769943));
#13219=CARTESIAN_POINT('',(0.001457106781,-0.00209439510510336,0.00799999999910028));
#13220=CARTESIAN_POINT('',(0.001457106781,-3.43669111491311E-12,0.008));
#13221=CARTESIAN_POINT('',(0.001457106781,-2.7183457229373E-12,0.008));
#13222=CARTESIAN_POINT('',(0.001457107156,-2.28165122079125E-12,-0.008));
#13223=CARTESIAN_POINT('',(0.001457106781,0.,9.68154981406677E-19));
#13224=CARTESIAN_POINT('',(-0.00374999999987468,1.93364582630688E-13,-2.28558934437229E-19));
#13225=CARTESIAN_POINT('',(-0.00375,0.,0.));
#13226=CARTESIAN_POINT('',(-0.00374999987527851,-1.8459280570297E-12,-0.00899999999987672));
#13227=CARTESIAN_POINT('',(-0.00374999987527851,-1.22168301791654E-12,0.00899999999987672));
#13228=CARTESIAN_POINT('',(-0.00375000000055703,-1.22168309480298E-12,0.00899999999975343));
#13229=CARTESIAN_POINT('',(-0.00375000000055552,-0.00117809724617388,0.00899999999961883));
#13230=CARTESIAN_POINT('',(-0.00375000000055249,-0.00353374253293338,0.00853138684369092));
#13231=CARTESIAN_POINT('',(-0.00375000000054865,-0.0065296606176239,0.00652964080030454));
#13232=CARTESIAN_POINT('',(-0.00375000000054607,-0.00853138118227796,0.00353381613659912));
#13233=CARTESIAN_POINT('',(-0.00375000000054517,-0.00923430940871994,3.20239732450106E-13));
#13234=CARTESIAN_POINT('',(-0.00375000000054607,-0.00853138118252307,-0.00353381613600736));
#13235=CARTESIAN_POINT('',(-0.00375000000054865,-0.0065296606180768,-0.00652964079985164));
#13236=CARTESIAN_POINT('',(-0.00375000000055249,-0.00353374253352514,-0.00853138684344582));
#13237=CARTESIAN_POINT('',(-0.00375000000055552,-0.00117809724679812,-0.00899999999953711));
#13238=CARTESIAN_POINT('',(-0.00375000000055703,-1.845925958314E-12,-0.00899999999975343));
#13239=CARTESIAN_POINT('',(0.0014571067816285,-5.47396505703968E-13,6.65202876568241E-20));
#13240=CARTESIAN_POINT('',(0.00110355339071671,1.58556738773517E-17,0.00814644660952611));
#13241=CARTESIAN_POINT('',(0.00119611345182742,2.63259265651322E-16,0.00805388654805348));
#13242=CARTESIAN_POINT('',(0.00132620708739174,-1.64577341757993E-15,0.00799999999964119));
#13243=CARTESIAN_POINT('',(0.0014571067814045,1.67659206997871E-17,0.00799999999958255));
#13244=CARTESIAN_POINT('',(0.00110355330247001,-2.9115133713822E-12,0.0081464466976514));
#13245=CARTESIAN_POINT('',(0.00110355339071671,-1.6708634304086E-12,-0.00814644660952611));
#13246=CARTESIAN_POINT('',(0.00110355339048919,-0.00213273473648634,-0.00814644660922211));
#13247=CARTESIAN_POINT('',(0.00110355339003597,-0.0063812246085619,-0.0063836502643864));
#13248=CARTESIAN_POINT('',(0.00110355338975351,-0.00902905761052969,-6.87539018106074E-13));
#13249=CARTESIAN_POINT('',(0.00110355339003597,-0.00638122460953407,0.00638365026341459));
#13250=CARTESIAN_POINT('',(0.00110355339048919,-0.00213273473772698,0.00814644660889731));
#13251=CARTESIAN_POINT('',(0.00110355339071671,-2.91151058367133E-12,0.00814644660952611));
#13252=CARTESIAN_POINT('',(0.00110355330262237,-1.67086175802321E-12,-0.00814644669762802));
#13253=CARTESIAN_POINT('',(0.0014571067814045,-3.13787920007409E-17,-0.00799999999958255));
#13254=CARTESIAN_POINT('',(0.00132620708739174,-1.66845701558407E-15,-0.00799999999964119));
#13255=CARTESIAN_POINT('',(0.00119611345182742,2.65760905900004E-16,-0.00805388654805348));
#13256=CARTESIAN_POINT('',(0.00110355339071671,4.46112367465754E-17,-0.00814644660952611));
#13257=CARTESIAN_POINT('',(0.0014571067816285,5.47397208070073E-13,-5.45798719985721E-19));
#13258=CARTESIAN_POINT('',(0.00110355339112794,0.,-1.04204690494148E-15));
#13259=CARTESIAN_POINT('',(-0.007263258046,0.,0.));
#13260=CARTESIAN_POINT('',(-0.003116025404,-3.86627750427725E-12,0.009));
#13261=CARTESIAN_POINT('',(-0.003116025404,-0.00117809724855378,0.0089999999994939));
#13262=CARTESIAN_POINT('',(-0.003116025404,-0.00353374253463681,0.00853138684304964));
#13263=CARTESIAN_POINT('',(-0.003116025404,-0.00652966061829104,0.00652964079963258));
#13264=CARTESIAN_POINT('',(-0.003116025404,-0.00853138118227268,0.00353381613649351));
#13265=CARTESIAN_POINT('',(-0.003116025404,-0.00923430940865992,1.06481072844012E-12));
#13266=CARTESIAN_POINT('',(-0.003116025404,-0.00853138118308765,-0.003533816134526));
#13267=CARTESIAN_POINT('',(-0.003116025404,-0.00652966061979692,-0.0065296407981267));
#13268=CARTESIAN_POINT('',(-0.003116025404,-0.00353374253660432,-0.00853138684223469));
#13269=CARTESIAN_POINT('',(-0.003116025404,-0.00117809725062936,-0.00899999999922221));
#13270=CARTESIAN_POINT('',(-0.003116025404,-5.9418618994418E-12,-0.009));
#13271=CARTESIAN_POINT('',(-0.00311602552873704,-1.84592937600593E-12,-0.00899999999997601));
#13272=CARTESIAN_POINT('',(-0.00311602552873704,1.12499936185184E-12,0.00899999999997601));
#13273=CARTESIAN_POINT('',(-0.003116025404,0.,0.));
#13274=CARTESIAN_POINT('',(0.00925000000025689,0.,-1.03355916846639E-15));
#13275=CARTESIAN_POINT('',(0.000896446609127943,0.,-1.04226268832191E-15));
#13276=CARTESIAN_POINT('',(0.000896446947516299,-2.38248677279272E-12,-0.00835355305274167));
#13277=CARTESIAN_POINT('',(0.000896446609127934,-2.83848445413882E-12,0.00835355339112793));
#13278=CARTESIAN_POINT('',(0.000896446609127957,-5.51507340218912E-12,-0.00835355339113002));
#13279=CARTESIAN_POINT('',(0.000896446609127957,-0.00109347758700829,-0.0083535533904081));
#13280=CARTESIAN_POINT('',(0.000896446609127956,-0.00327992299444752,-0.00791859949855468));
#13281=CARTESIAN_POINT('',(0.000896446609127955,-0.00606065206815843,-0.00606063367022831));
#13282=CARTESIAN_POINT('',(0.000896446609127951,-0.00791859424588842,-0.00327999130602281));
#13283=CARTESIAN_POINT('',(0.000896446609127948,-0.00857103296393836,9.87285581686735E-13));
#13284=CARTESIAN_POINT('',(0.000896446609127945,-0.00791859424513199,0.00327999130784692));
#13285=CARTESIAN_POINT('',(0.000896446609127942,-0.00606065206676072,0.00606063367162394));
#13286=CARTESIAN_POINT('',(0.00089644660912794,-0.00327992299262134,0.00791859949930901));
#13287=CARTESIAN_POINT('',(0.000896446609127939,-0.00109347758508179,0.00835355339065819));
#13288=CARTESIAN_POINT('',(0.000896446609127939,-3.58857283965566E-12,0.00835355339112793));
#13289=CARTESIAN_POINT('',(-0.00311602540366083,1.89369138590977E-13,4.60164670987285E-19));
#13290=CARTESIAN_POINT('',(-0.00311602540347409,-2.08135904343245E-17,0.00899999999995202));
#13291=CARTESIAN_POINT('',(-0.00276695955312565,-2.17671273402248E-15,0.00899999999988684));
#13292=CARTESIAN_POINT('',(-0.00242453292500672,-2.5821733949979E-16,0.00880229989405671));
#13293=CARTESIAN_POINT('',(-0.00224999999965417,-1.04806440198648E-18,0.0085000000001643));
#13294=CARTESIAN_POINT('',(-0.00224999987482708,-1.83738466424475E-19,0.00850000000008215));
#13295=CARTESIAN_POINT('',(-0.00224999999965417,2.2030464917804E-13,4.66825340357479E-19));
#13296=CARTESIAN_POINT('',(-0.00224999987482708,-1.74337942337899E-12,-0.00850000000008215));
#13297=CARTESIAN_POINT('',(-0.00224999999965417,-1.44542388119606E-17,-0.0085000000001643));
#13298=CARTESIAN_POINT('',(-0.00242453292500672,-2.56372140876474E-16,-0.00880229989405671));
#13299=CARTESIAN_POINT('',(-0.00276695955312565,-2.15760081618848E-15,-0.00899999999988684));
#13300=CARTESIAN_POINT('',(-0.00311602540347409,1.49516727692217E-17,-0.00899999999995202));
#13301=CARTESIAN_POINT('',(-0.00311602540366083,-1.89369495587902E-13,-4.56753702428283E-19));
#13302=CARTESIAN_POINT('',(-0.00224999999965417,-1.74337645012797E-12,-0.0085000000001643));
#13303=CARTESIAN_POINT('',(-0.00224999999969392,-0.00111264739985699,-0.00849999999996493));
#13304=CARTESIAN_POINT('',(-0.00224999999977339,-0.00333742350419627,-0.00805742090804886));
#13305=CARTESIAN_POINT('',(-0.00224999999987446,-0.00616690169538636,-0.00616688297774479));
#13306=CARTESIAN_POINT('',(-0.002249999999942,-0.00805741556187121,-0.00333749301710294));
#13307=CARTESIAN_POINT('',(-0.00224999999996571,-0.00872129221981244,8.94381676439934E-13));
#13308=CARTESIAN_POINT('',(-0.002249999999942,-0.00805741556118667,0.00333749301875555));
#13309=CARTESIAN_POINT('',(-0.00224999999987446,-0.00616690169412152,0.00616688297900963));
#13310=CARTESIAN_POINT('',(-0.00224999999977339,-0.00333742350254365,0.00805742090873338));
#13311=CARTESIAN_POINT('',(-0.00224999999969392,-0.00111264739811362,0.00850000000019314));
#13312=CARTESIAN_POINT('',(-0.00224999999965417,-1.35791309261817E-17,0.0085000000001643));
#13313=CARTESIAN_POINT('',(0.000542893218371495,5.47403523416524E-13,1.10783975326665E-19));
#13314=CARTESIAN_POINT('',(0.000896446609283292,-1.46288588890009E-17,0.0083535533904739));
#13315=CARTESIAN_POINT('',(0.000803886548172581,-5.03456191566966E-16,0.00844611345194653));
#13316=CARTESIAN_POINT('',(0.00067379291260826,-1.94773245151004E-15,0.00850000000035882));
#13317=CARTESIAN_POINT('',(0.000542893218595496,1.69082711704543E-17,0.00850000000041746));
#13318=CARTESIAN_POINT('',(0.000542893093797748,-2.12500021499821E-12,0.00850000000020873));
#13319=CARTESIAN_POINT('',(0.000542893218595496,-2.12499836668962E-12,0.00850000000041746));
#13320=CARTESIAN_POINT('',(0.000542893218721609,-0.00111264740011923,0.00850000000006764));
#13321=CARTESIAN_POINT('',(0.000542893218973776,-0.00333742350416026,0.00805742090796045));
#13322=CARTESIAN_POINT('',(0.000542893219294483,-0.00616690169492879,0.00616688297771508));
#13323=CARTESIAN_POINT('',(0.000542893219508763,-0.00805741556119902,0.00333749301739052));
#13324=CARTESIAN_POINT('',(0.00054289321958401,-0.00872129221924304,-1.95784323807277E-13));
#13325=CARTESIAN_POINT('',(0.000542893219508763,-0.00805741556104918,-0.00333749301775226));
#13326=CARTESIAN_POINT('',(0.000542893219294483,-0.00616690169465192,-0.00616688297799194));
#13327=CARTESIAN_POINT('',(0.000542893218973777,-0.00333742350379851,-0.00805742090811029));
#13328=CARTESIAN_POINT('',(0.000542893218721609,-0.00111264739973761,-0.0085000000001176));
#13329=CARTESIAN_POINT('',(0.000542893218595496,-1.74337804822321E-12,-0.00850000000041746));
#13330=CARTESIAN_POINT('',(0.000542893093922748,-1.7433764476282E-12,-0.00850000000020873));
#13331=CARTESIAN_POINT('',(0.000542893218595496,1.61471761803093E-18,-0.00850000000041746));
#13332=CARTESIAN_POINT('',(0.000673792912608261,-1.96176775230103E-15,-0.00850000000035882));
#13333=CARTESIAN_POINT('',(0.000803886548172583,-5.16138536658815E-16,-0.00844611345194653));
#13334=CARTESIAN_POINT('',(0.000896446609283294,-2.59491966845735E-17,-0.0083535533904739));
#13335=CARTESIAN_POINT('',(0.000542893218371494,-5.47404119942789E-13,5.87721542220263E-20));
#13336=CARTESIAN_POINT('',(0.000542893218595497,-5.47404119968178E-13,5.87721541987024E-20));
#13337=CARTESIAN_POINT('',(-0.007263258046,0.,2.44324620272917E-53));
#13338=CARTESIAN_POINT('',(0.0175000000000004,0.06775,1.10617214860196E-34));
#13339=CARTESIAN_POINT('',(0.00420000000011192,-3.50899506067413E-13,5.47386837469071E-19));
#13340=CARTESIAN_POINT('',(0.00420000000019215,-2.46124009164679E-12,0.0120000000003955));
#13341=CARTESIAN_POINT('',(0.00420000000019962,-0.00157079632905111,0.0120000000000274));
#13342=CARTESIAN_POINT('',(0.00420000000021455,-0.00471165671129617,0.0113751824584622));
#13343=CARTESIAN_POINT('',(0.00420000000023355,-0.00870621415729384,0.00870618773365808));
#13344=CARTESIAN_POINT('',(0.00420000000024625,-0.0113751749099263,0.00471175484862072));
#13345=CARTESIAN_POINT('',(0.00420000000025071,-0.0123124125450508,2.76378563580788E-13));
#13346=CARTESIAN_POINT('',(0.00420000000024625,-0.0113751749101378,-0.00471175484810999));
#13347=CARTESIAN_POINT('',(0.00420000000023355,-0.00870621415768473,-0.00870618773326719));
#13348=CARTESIAN_POINT('',(0.00420000000021456,-0.0047116567118069,-0.0113751824582506));
#13349=CARTESIAN_POINT('',(0.00420000000019962,-0.00157079632958987,-0.0119999999999568));
#13350=CARTESIAN_POINT('',(0.00420000000019215,-3.00000140206592E-12,-0.0120000000003955));
#13351=CARTESIAN_POINT('',(0.00419999987509607,-2.46123887461207E-12,0.0120000000001977));
#13352=CARTESIAN_POINT('',(0.00419999987509607,-3.00000082519295E-12,-0.0120000000001977));
#13353=CARTESIAN_POINT('',(0.00420000000019215,-3.50899506067795E-13,5.47386837468749E-19));
#13354=CARTESIAN_POINT('',(0.00450000000033692,-3.52326344841177E-13,5.4618554526698E-19));
#13355=CARTESIAN_POINT('',(0.00450000000039257,0.0116999999998398,5.4618554526698E-19));
#13356=CARTESIAN_POINT('',(0.0045,-5.3776427755281E-19,-1.47451495458029E-19));
#13357=CARTESIAN_POINT('',(0.0045,0.,-3.14458944017069E-18));
#13358=CARTESIAN_POINT('',(0.0045,0.,-0.01065));
#13359=CARTESIAN_POINT('',(-0.0206375,0.,-4.67643299434448E-52));
#13360=CARTESIAN_POINT('',(-0.0042,-5.15503667236967E-12,-0.012));
#13361=CARTESIAN_POINT('',(-0.0042,-0.00157079633140504,-0.0119999999993252));
#13362=CARTESIAN_POINT('',(-0.0042,-0.00471165671284908,-0.0113751824573995));
#13363=CARTESIAN_POINT('',(-0.0042,-0.0087062141577214,-0.00870618773284344));
#13364=CARTESIAN_POINT('',(-0.0042,-0.0113751749096969,-0.00471175484865801));
#13365=CARTESIAN_POINT('',(-0.0042,-0.0123124125448799,-1.41974949723703E-12));
#13366=CARTESIAN_POINT('',(-0.0042,-0.0113751749107835,0.00471175484603467));
#13367=CARTESIAN_POINT('',(-0.0042,-0.00870621415972922,0.0087061877308356));
#13368=CARTESIAN_POINT('',(-0.0042,-0.00471165671547242,0.0113751824563129));
#13369=CARTESIAN_POINT('',(-0.0042,-0.00157079633417248,0.0119999999989629));
#13370=CARTESIAN_POINT('',(-0.0042,-7.92248253258906E-12,0.012));
#13371=CARTESIAN_POINT('',(-0.00419999987509607,-2.46123798780892E-12,0.0120000000001977));
#13372=CARTESIAN_POINT('',(-0.004199999875,-4.0775188822195E-12,-0.012));
#13373=CARTESIAN_POINT('',(-0.0042,0.,-1.2166193978184E-18));
#13374=CARTESIAN_POINT('',(-0.0206375,0.,0.));
#13375=CARTESIAN_POINT('',(0.00100623059,-4.57509504672808E-12,-0.01065));
#13376=CARTESIAN_POINT('',(0.00100623059,-0.00139408174412197,-0.0106499999994011));
#13377=CARTESIAN_POINT('',(0.00100623059,-0.00418159533265356,-0.0100954744309421));
#13378=CARTESIAN_POINT('',(0.00100623059,-0.00772676506497774,-0.00772674161289855));
#13379=CARTESIAN_POINT('',(0.00100623059,-0.010095467732356,-0.00418168242818399));
#13380=CARTESIAN_POINT('',(0.00100623059,-0.0109272661335809,-1.26002854163711E-12));
#13381=CARTESIAN_POINT('',(0.00100623059,-0.0100954677333204,0.00418168242585576));
#13382=CARTESIAN_POINT('',(0.00100623059,-0.00772676506675968,0.0077267416111166));
#13383=CARTESIAN_POINT('',(0.00100623059,-0.00418159533498178,0.0100954744299777));
#13384=CARTESIAN_POINT('',(0.00100623059,-0.00139408174657808,0.0106499999990796));
#13385=CARTESIAN_POINT('',(0.00100623059,-7.03120324767279E-12,0.01065));
#13386=CARTESIAN_POINT('',(0.00100623096506661,-2.18434900175713E-12,0.0106499999996362));
#13387=CARTESIAN_POINT('',(0.00100623059006661,-4.95004771836549E-12,-0.0106499999996362));
#13388=CARTESIAN_POINT('',(0.00100623059013322,-5.59151227703387E-14,4.31770786296025E-20));
#13389=CARTESIAN_POINT('',(-0.00420000000011192,-3.50900396996374E-13,-2.29851109841953E-19));
#13390=CARTESIAN_POINT('',(-0.00450000000033692,-3.52327230154582E-13,-2.37871579129804E-19));
#13391=CARTESIAN_POINT('',(-0.00450000000039257,0.0116999999998398,-2.37871579129804E-19));
#13392=CARTESIAN_POINT('',(1.154356125671E-13,4.73423576231519E-14,5.99501471359368E-21));
#13393=CARTESIAN_POINT('',(0.00100623059013322,5.05895643960993E-20,-0.0106499999992724));
#13394=CARTESIAN_POINT('',(0.00132239692493253,3.43168701089793E-15,-0.0102965152906072));
#13395=CARTESIAN_POINT('',(0.00153614706478366,8.87052617196055E-15,-0.00923383493259741));
#13396=CARTESIAN_POINT('',(0.000724069227561596,4.32262384432489E-15,-0.00851584589933923));
#13397=CARTESIAN_POINT('',(0.000258602131639666,7.10249954130499E-18,-0.00842500002362359));
#13398=CARTESIAN_POINT('',(0.000258602136233779,-2.86275794301951E-12,-0.00842500000008472));
#13399=CARTESIAN_POINT('',(0.000258602011467558,-2.86275710191455E-12,-0.00842500000016943));
#13400=CARTESIAN_POINT('',(0.000258602011476953,-0.00110282992379344,-0.00842499999978821));
#13401=CARTESIAN_POINT('',(0.00025860201149574,-0.0033079756503873,-0.00798632601725331));
#13402=CARTESIAN_POINT('',(0.000258602011519631,-0.00611248785699539,-0.00611246930397495));
#13403=CARTESIAN_POINT('',(0.000258602011535596,-0.00798632071841419,-0.00330804454916419));
#13404=CARTESIAN_POINT('',(0.000258602011541202,-0.00864433964108412,5.82148394867342E-13));
#13405=CARTESIAN_POINT('',(0.000258602011535596,-0.00798632071796863,0.00330804455023986));
#13406=CARTESIAN_POINT('',(0.000258602011519632,-0.00611248785617209,0.00611246930479825));
#13407=CARTESIAN_POINT('',(0.000258602011495739,-0.00330797564931162,0.00798632601769886));
#13408=CARTESIAN_POINT('',(0.000258602011476953,-0.00110282992265868,0.00842499999993675));
#13409=CARTESIAN_POINT('',(0.000258602011467558,-1.72799521891854E-12,0.00842500000016943));
#13410=CARTESIAN_POINT('',(0.000258602136233782,-1.72799408318983E-12,0.00842500000008472));
#13411=CARTESIAN_POINT('',(0.000258602131639668,-2.26363092258843E-17,0.00842500002362359));
#13412=CARTESIAN_POINT('',(0.000724069186718163,4.30004688906155E-15,0.00851584589136776));
#13413=CARTESIAN_POINT('',(0.00153614696900967,8.86942973976054E-15,0.00923383480668362));
#13414=CARTESIAN_POINT('',(0.00132239699826857,3.44075559505266E-15,0.0102965150770454));
#13415=CARTESIAN_POINT('',(0.00100623075658947,1.92149073831785E-17,0.0106499998131686));
#13416=CARTESIAN_POINT('',(1.1543600703228E-13,-4.73427093034189E-14,5.83742937136908E-20));
#13417=CARTESIAN_POINT('',(0.00025860201146756,-4.95458259515107E-14,5.44685981140106E-20));
#13418=CARTESIAN_POINT('',(-0.0045,-5.3776427755281E-19,1.47451495458029E-19));
#13419=CARTESIAN_POINT('',(-0.0045,0.,0.));
#13420=CARTESIAN_POINT('',(-0.0045,0.,-0.011075));
#13421=CARTESIAN_POINT('',(-0.0206375,0.,-9.16300179894287E-52));
#13422=CARTESIAN_POINT('',(0.0045,0.,-1.98752982420284E-18));
#13423=CARTESIAN_POINT('',(0.0045,0.,-0.008425));
#13424=CARTESIAN_POINT('',(-0.0206375,0.,0.));
#13425=CARTESIAN_POINT('',(-0.000258602011,-7.31179117070199E-12,0.011075));
#13426=CARTESIAN_POINT('',(-0.000258602011,-0.00144971411674669,0.0110749999990429));
#13427=CARTESIAN_POINT('',(-0.000258602011,-0.00434846651032143,0.0104983454753055));
#13428=CARTESIAN_POINT('',(-0.000258602011,-0.00803511015158343,0.00803508575991702));
#13429=CARTESIAN_POINT('',(-0.000258602011,-0.0104983385114106,0.00434855707665283));
#13430=CARTESIAN_POINT('',(-0.000258602011,-0.0113633307445454,-1.31030853718747E-12));
#13431=CARTESIAN_POINT('',(-0.000258602011,-0.0104983385104078,-0.00434855707907396));
#13432=CARTESIAN_POINT('',(-0.000258602011,-0.00803511014973037,-0.00803508576177009));
#13433=CARTESIAN_POINT('',(-0.000258602011,-0.0043484665079003,-0.0104983454763083));
#13434=CARTESIAN_POINT('',(-0.000258602011,-0.00144971411419257,-0.0110749999993772));
#13435=CARTESIAN_POINT('',(-0.000258602011,-4.75766926220784E-12,-0.011075));
#13436=CARTESIAN_POINT('',(-0.00025860238623378,-9.94454622315446E-13,-0.0110749999999153));
#13437=CARTESIAN_POINT('',(-0.000258602071199268,-6.4246432521501E-12,0.0110749999882117));
#13438=CARTESIAN_POINT('',(-0.000258602011467561,4.51272795225522E-14,-3.71516306442422E-19));
#13439=CARTESIAN_POINT('',(0.0045,-2.22911966663019E-18,1.73472347597681E-20));
#13440=CARTESIAN_POINT('',(0.00450000000033692,3.48751202232752E-13,1.08129136841049E-19));
#13441=CARTESIAN_POINT('',(0.00450000000033692,6.37547546112859E-19,0.00779999999980785));
#13442=CARTESIAN_POINT('',(0.00450000000036139,-1.95000042881955E-12,-0.00779999999974705));
#13443=CARTESIAN_POINT('',(0.00450000000033692,-3.48751060863252E-13,-4.06296004640648E-19));
#13444=CARTESIAN_POINT('',(-1.1543990834159E-13,-4.73314002437894E-14,3.54060453998605E-19));
#13445=CARTESIAN_POINT('',(-0.0010062306454784,7.00818953022586E-18,-0.00885000006260538));
#13446=CARTESIAN_POINT('',(-0.00132239692205273,3.80617846662212E-15,-0.00920348474991875));
#13447=CARTESIAN_POINT('',(-0.00153614703263649,9.26191304452231E-15,-0.0102661649538024));
#13448=CARTESIAN_POINT('',(-0.000724069398158462,4.2080152504004E-15,-0.0109841539795411));
#13449=CARTESIAN_POINT('',(-0.000258602372466113,5.89741576151065E-17,-0.0110749999293739));
#13450=CARTESIAN_POINT('',(-0.00100623071506661,-7.94670107870803E-13,-0.0088500000003638));
#13451=CARTESIAN_POINT('',(-0.000258602011467561,1.98785142045412E-17,0.0110749999998306));
#13452=CARTESIAN_POINT('',(-0.000724069122077457,4.17825833481557E-15,0.0109841541650723));
#13453=CARTESIAN_POINT('',(-0.00153614703309098,9.25202015462542E-15,0.0102661651868448));
#13454=CARTESIAN_POINT('',(-0.00132239696292048,3.81144573458941E-15,0.0092034847956103));
#13455=CARTESIAN_POINT('',(-0.0010062306454784,1.90012882174815E-17,0.00885000006260538));
#13456=CARTESIAN_POINT('',(-0.00100623071506661,-6.59462196535367E-12,0.0088500000003638));
#13457=CARTESIAN_POINT('',(-0.00100623059013322,-6.59462086751533E-12,0.00885000000072759));
#13458=CARTESIAN_POINT('',(-0.00100623059014309,-0.00115846229739644,0.00884999999986943));
#13459=CARTESIAN_POINT('',(-0.00100623059016283,-0.00347484682895264,0.0083891970618622));
#13460=CARTESIAN_POINT('',(-0.00100623059018793,-0.0064208329443351,0.00642081345110636));
#13461=CARTESIAN_POINT('',(-0.00100623059020469,-0.00838919149809096,0.00347491919774606));
#13462=CARTESIAN_POINT('',(-0.00100623059021058,-0.00908040425267338,-2.97546799044951E-12));
#13463=CARTESIAN_POINT('',(-0.00100623059020469,-0.00838919149581363,-0.00347491920324402));
#13464=CARTESIAN_POINT('',(-0.00100623059018793,-0.00642083294012714,-0.00642081345531434));
#13465=CARTESIAN_POINT('',(-0.00100623059016283,-0.00347484682345468,-0.00838919706413948));
#13466=CARTESIAN_POINT('',(-0.00100623059014309,-0.00115846229159649,-0.00885000000062864));
#13467=CARTESIAN_POINT('',(-0.00100623059013322,-7.94669450589741E-13,-0.00885000000072759));
#13468=CARTESIAN_POINT('',(-1.1544007415132E-13,4.73304495273867E-14,-3.69660968558101E-19));
#13469=CARTESIAN_POINT('',(-0.00100623059013322,3.87578284472844E-14,-3.76880161186426E-19));
#13470=CARTESIAN_POINT('',(0.00420000000011192,-3.50891387635993E-13,-4.14898835309052E-19));
#13471=CARTESIAN_POINT('',(0.00420000000019215,8.38119770267861E-18,0.00749999999960454));
#13472=CARTESIAN_POINT('',(0.00435707963295547,-4.05846340527414E-15,0.00749999999964655));
#13473=CARTESIAN_POINT('',(0.00450000000032556,-1.62862306384024E-15,0.00764292036704453));
#13474=CARTESIAN_POINT('',(0.00450000000033692,-3.54563742746683E-19,0.00779999999980785));
#13475=CARTESIAN_POINT('',(0.00419999987517108,-1.5382740212674E-12,0.00749999999980227));
#13476=CARTESIAN_POINT('',(0.00450000000033692,-1.43886481780106E-17,-0.00779999999980785));
#13477=CARTESIAN_POINT('',(0.00450000000032556,-1.62909625669243E-15,-0.00764292036704453));
#13478=CARTESIAN_POINT('',(0.00435707963295547,-4.04642258766554E-15,-0.00749999999964655));
#13479=CARTESIAN_POINT('',(0.00420000000019215,3.31895800936513E-17,-0.00749999999960454));
#13480=CARTESIAN_POINT('',(0.00419999987509607,-4.29142485976802E-12,-0.00749999999980227));
#13481=CARTESIAN_POINT('',(0.00420000000019215,-4.29142066913366E-12,-0.00749999999960454));
#13482=CARTESIAN_POINT('',(0.00420000000020615,-0.00196349541225418,-0.00749999999857291));
#13483=CARTESIAN_POINT('',(0.00420000000023406,-0.0058748540154159,-0.00587708718402969));
#13484=CARTESIAN_POINT('',(0.00420000000025145,-0.00831257299276455,1.52571835373982E-12));
#13485=CARTESIAN_POINT('',(0.00420000000023406,-0.0058748540132585,0.00587708718618627));
#13486=CARTESIAN_POINT('',(0.00420000000020615,-0.00196349540950103,0.00749999999929369));
#13487=CARTESIAN_POINT('',(0.00420000000019215,-1.53826945716326E-12,0.00749999999960454));
#13488=CARTESIAN_POINT('',(0.00420000000011192,3.50891535870921E-13,1.16083160393565E-19));
#13489=CARTESIAN_POINT('',(0.00420000000011192,3.50891535870921E-13,1.16083160393565E-19));
#13490=CARTESIAN_POINT('',(-0.0206375,0.,0.));
#13491=CARTESIAN_POINT('',(-0.0045,0.,0.));
#13492=CARTESIAN_POINT('',(-0.0045,0.,-0.00885));
#13493=CARTESIAN_POINT('',(-0.0206375,0.,-2.47065262083525E-51));
#13494=CARTESIAN_POINT('',(-0.0042,-3.22189792023104E-12,-0.0075));
#13495=CARTESIAN_POINT('',(-0.0042,-0.0019634954110344,-0.00749999999915651));
#13496=CARTESIAN_POINT('',(-0.0042,-0.00587485401406066,-0.00587708718534322));
#13497=CARTESIAN_POINT('',(-0.0042,-0.00831257299263083,-9.5852737806285E-13));
#13498=CARTESIAN_POINT('',(-0.0042,-0.00587485401541604,0.00587708718398836));
#13499=CARTESIAN_POINT('',(-0.0042,-0.00196349541276405,0.00749999999870368));
#13500=CARTESIAN_POINT('',(-0.0042,-4.95155158286816E-12,0.0075));
#13501=CARTESIAN_POINT('',(-0.00419999962509607,-1.53827397134479E-12,0.00749999999980227));
#13502=CARTESIAN_POINT('',(-0.00420000000009607,-3.48594912388589E-12,-0.00749999999980227));
#13503=CARTESIAN_POINT('',(-0.00420000000011191,3.50891751372691E-13,2.79083595183788E-19));
#13504=CARTESIAN_POINT('',(-0.0045,-4.07660016854549E-19,-7.28583859910259E-19));
#13505=CARTESIAN_POINT('',(-0.00450000000033692,3.48751417212871E-13,2.87745340681233E-19));
#13506=CARTESIAN_POINT('',(-0.00450000000033692,-2.42388042693057E-19,-0.00779999999980785));
#13507=CARTESIAN_POINT('',(-0.00450000000036139,-1.9500002825196E-12,0.00779999999974705));
#13508=CARTESIAN_POINT('',(-0.00450000000033692,-3.48750946764454E-13,-1.41700427235676E-19));
#13509=CARTESIAN_POINT('',(-0.00420000000011191,-3.50891287789699E-13,-1.29656749332468E-19));
#13510=CARTESIAN_POINT('',(-0.00450000000033692,-2.40464944123498E-19,0.00779999999980786));
#13511=CARTESIAN_POINT('',(-0.00450000000032556,-1.62850896504167E-15,0.00764292036704453));
#13512=CARTESIAN_POINT('',(-0.00435707963295547,-4.05835609638575E-15,0.00749999999964656));
#13513=CARTESIAN_POINT('',(-0.00420000000019214,8.48104399744249E-18,0.00749999999960455));
#13514=CARTESIAN_POINT('',(-0.00420000000019214,3.32894263884152E-17,-0.00749999999960455));
#13515=CARTESIAN_POINT('',(-0.00435707963295547,-4.04631527877715E-15,-0.00749999999964656));
#13516=CARTESIAN_POINT('',(-0.00450000000032556,-1.62898215789386E-15,-0.00764292036704453));
#13517=CARTESIAN_POINT('',(-0.00450000000033692,-1.42745493793874E-17,-0.00779999999980786));
#13518=CARTESIAN_POINT('',(-0.00420000000011191,3.50891751372691E-13,2.79083595183788E-19));
#13519=CARTESIAN_POINT('',(0.0175000000000005,-0.058,-3.31955057691157E-34));
#13520=CARTESIAN_POINT('',(0.00420000000011192,-3.50899506067413E-13,5.47386837469071E-19));
#13521=CARTESIAN_POINT('',(0.00420000000019215,-2.46124009164679E-12,0.0120000000003955));
#13522=CARTESIAN_POINT('',(0.00420000000019962,-0.00157079632905111,0.0120000000000274));
#13523=CARTESIAN_POINT('',(0.00420000000021455,-0.00471165671129617,0.0113751824584622));
#13524=CARTESIAN_POINT('',(0.00420000000023355,-0.00870621415729384,0.00870618773365808));
#13525=CARTESIAN_POINT('',(0.00420000000024625,-0.0113751749099263,0.00471175484862072));
#13526=CARTESIAN_POINT('',(0.00420000000025071,-0.0123124125450508,2.76378563580788E-13));
#13527=CARTESIAN_POINT('',(0.00420000000024625,-0.0113751749101378,-0.00471175484810999));
#13528=CARTESIAN_POINT('',(0.00420000000023355,-0.00870621415768473,-0.00870618773326719));
#13529=CARTESIAN_POINT('',(0.00420000000021456,-0.0047116567118069,-0.0113751824582506));
#13530=CARTESIAN_POINT('',(0.00420000000019962,-0.00157079632958987,-0.0119999999999568));
#13531=CARTESIAN_POINT('',(0.00420000000019215,-3.00000140206592E-12,-0.0120000000003955));
#13532=CARTESIAN_POINT('',(0.00419999987509607,-2.46123887461207E-12,0.0120000000001977));
#13533=CARTESIAN_POINT('',(0.00419999987509607,-3.00000082519295E-12,-0.0120000000001977));
#13534=CARTESIAN_POINT('',(0.00420000000019215,-3.50899506067795E-13,5.47386837468749E-19));
#13535=CARTESIAN_POINT('',(0.00450000000033692,-3.52326344841177E-13,5.4618554526698E-19));
#13536=CARTESIAN_POINT('',(0.00450000000039257,0.0116999999998398,5.4618554526698E-19));
#13537=CARTESIAN_POINT('',(0.0045,-5.3776427755281E-19,-1.47451495458029E-19));
#13538=CARTESIAN_POINT('',(0.0045,0.,-3.14458944017069E-18));
#13539=CARTESIAN_POINT('',(0.0045,0.,-0.01065));
#13540=CARTESIAN_POINT('',(-0.0206375,0.,-4.67643299434448E-52));
#13541=CARTESIAN_POINT('',(-0.0042,-5.15503667236967E-12,-0.012));
#13542=CARTESIAN_POINT('',(-0.0042,-0.00157079633140504,-0.0119999999993252));
#13543=CARTESIAN_POINT('',(-0.0042,-0.00471165671284908,-0.0113751824573995));
#13544=CARTESIAN_POINT('',(-0.0042,-0.0087062141577214,-0.00870618773284344));
#13545=CARTESIAN_POINT('',(-0.0042,-0.0113751749096969,-0.00471175484865801));
#13546=CARTESIAN_POINT('',(-0.0042,-0.0123124125448799,-1.41974949723703E-12));
#13547=CARTESIAN_POINT('',(-0.0042,-0.0113751749107835,0.00471175484603467));
#13548=CARTESIAN_POINT('',(-0.0042,-0.00870621415972922,0.0087061877308356));
#13549=CARTESIAN_POINT('',(-0.0042,-0.00471165671547242,0.0113751824563129));
#13550=CARTESIAN_POINT('',(-0.0042,-0.00157079633417248,0.0119999999989629));
#13551=CARTESIAN_POINT('',(-0.0042,-7.92248253258906E-12,0.012));
#13552=CARTESIAN_POINT('',(-0.00419999987509607,-2.46123798780892E-12,0.0120000000001977));
#13553=CARTESIAN_POINT('',(-0.004199999875,-4.0775188822195E-12,-0.012));
#13554=CARTESIAN_POINT('',(-0.0042,0.,-1.2166193978184E-18));
#13555=CARTESIAN_POINT('',(-0.0206375,0.,0.));
#13556=CARTESIAN_POINT('',(0.00100623059,-4.57509504672808E-12,-0.01065));
#13557=CARTESIAN_POINT('',(0.00100623059,-0.00139408174412197,-0.0106499999994011));
#13558=CARTESIAN_POINT('',(0.00100623059,-0.00418159533265356,-0.0100954744309421));
#13559=CARTESIAN_POINT('',(0.00100623059,-0.00772676506497774,-0.00772674161289855));
#13560=CARTESIAN_POINT('',(0.00100623059,-0.010095467732356,-0.00418168242818399));
#13561=CARTESIAN_POINT('',(0.00100623059,-0.0109272661335809,-1.26002854163711E-12));
#13562=CARTESIAN_POINT('',(0.00100623059,-0.0100954677333204,0.00418168242585576));
#13563=CARTESIAN_POINT('',(0.00100623059,-0.00772676506675968,0.0077267416111166));
#13564=CARTESIAN_POINT('',(0.00100623059,-0.00418159533498178,0.0100954744299777));
#13565=CARTESIAN_POINT('',(0.00100623059,-0.00139408174657808,0.0106499999990796));
#13566=CARTESIAN_POINT('',(0.00100623059,-7.03120324767279E-12,0.01065));
#13567=CARTESIAN_POINT('',(0.00100623096506661,-2.18434900175713E-12,0.0106499999996362));
#13568=CARTESIAN_POINT('',(0.00100623059006661,-4.95004771836549E-12,-0.0106499999996362));
#13569=CARTESIAN_POINT('',(0.00100623059013322,-5.59151227703387E-14,4.31770786296025E-20));
#13570=CARTESIAN_POINT('',(-0.00420000000011192,-3.50900396996374E-13,-2.29851109841953E-19));
#13571=CARTESIAN_POINT('',(-0.00450000000033692,-3.52327230154582E-13,-2.37871579129804E-19));
#13572=CARTESIAN_POINT('',(-0.00450000000039257,0.0116999999998398,-2.37871579129804E-19));
#13573=CARTESIAN_POINT('',(1.154356125671E-13,4.73423576231519E-14,5.99501471359368E-21));
#13574=CARTESIAN_POINT('',(0.00100623059013322,5.05895643960993E-20,-0.0106499999992724));
#13575=CARTESIAN_POINT('',(0.00132239692493253,3.43168701089793E-15,-0.0102965152906072));
#13576=CARTESIAN_POINT('',(0.00153614706478366,8.87052617196055E-15,-0.00923383493259741));
#13577=CARTESIAN_POINT('',(0.000724069227561596,4.32262384432489E-15,-0.00851584589933923));
#13578=CARTESIAN_POINT('',(0.000258602131639666,7.10249954130499E-18,-0.00842500002362359));
#13579=CARTESIAN_POINT('',(0.000258602136233779,-2.86275794301951E-12,-0.00842500000008472));
#13580=CARTESIAN_POINT('',(0.000258602011467558,-2.86275710191455E-12,-0.00842500000016943));
#13581=CARTESIAN_POINT('',(0.000258602011476953,-0.00110282992379344,-0.00842499999978821));
#13582=CARTESIAN_POINT('',(0.00025860201149574,-0.0033079756503873,-0.00798632601725331));
#13583=CARTESIAN_POINT('',(0.000258602011519631,-0.00611248785699539,-0.00611246930397495));
#13584=CARTESIAN_POINT('',(0.000258602011535596,-0.00798632071841419,-0.00330804454916419));
#13585=CARTESIAN_POINT('',(0.000258602011541202,-0.00864433964108412,5.82148394867342E-13));
#13586=CARTESIAN_POINT('',(0.000258602011535596,-0.00798632071796863,0.00330804455023986));
#13587=CARTESIAN_POINT('',(0.000258602011519632,-0.00611248785617209,0.00611246930479825));
#13588=CARTESIAN_POINT('',(0.000258602011495739,-0.00330797564931162,0.00798632601769886));
#13589=CARTESIAN_POINT('',(0.000258602011476953,-0.00110282992265868,0.00842499999993675));
#13590=CARTESIAN_POINT('',(0.000258602011467558,-1.72799521891854E-12,0.00842500000016943));
#13591=CARTESIAN_POINT('',(0.000258602136233782,-1.72799408318983E-12,0.00842500000008472));
#13592=CARTESIAN_POINT('',(0.000258602131639668,-2.26363092258843E-17,0.00842500002362359));
#13593=CARTESIAN_POINT('',(0.000724069186718163,4.30004688906155E-15,0.00851584589136776));
#13594=CARTESIAN_POINT('',(0.00153614696900967,8.86942973976054E-15,0.00923383480668362));
#13595=CARTESIAN_POINT('',(0.00132239699826857,3.44075559505266E-15,0.0102965150770454));
#13596=CARTESIAN_POINT('',(0.00100623075658947,1.92149073831785E-17,0.0106499998131686));
#13597=CARTESIAN_POINT('',(1.1543600703228E-13,-4.73427093034189E-14,5.83742937136908E-20));
#13598=CARTESIAN_POINT('',(0.00025860201146756,-4.95458259515107E-14,5.44685981140106E-20));
#13599=CARTESIAN_POINT('',(-0.0045,-5.3776427755281E-19,1.47451495458029E-19));
#13600=CARTESIAN_POINT('',(-0.0045,0.,0.));
#13601=CARTESIAN_POINT('',(-0.0045,0.,-0.011075));
#13602=CARTESIAN_POINT('',(-0.0206375,0.,-9.16300179894287E-52));
#13603=CARTESIAN_POINT('',(0.0045,0.,-1.98752982420284E-18));
#13604=CARTESIAN_POINT('',(0.0045,0.,-0.008425));
#13605=CARTESIAN_POINT('',(-0.0206375,0.,0.));
#13606=CARTESIAN_POINT('',(-0.000258602011,-7.31179117070199E-12,0.011075));
#13607=CARTESIAN_POINT('',(-0.000258602011,-0.00144971411674669,0.0110749999990429));
#13608=CARTESIAN_POINT('',(-0.000258602011,-0.00434846651032143,0.0104983454753055));
#13609=CARTESIAN_POINT('',(-0.000258602011,-0.00803511015158343,0.00803508575991702));
#13610=CARTESIAN_POINT('',(-0.000258602011,-0.0104983385114106,0.00434855707665283));
#13611=CARTESIAN_POINT('',(-0.000258602011,-0.0113633307445454,-1.31030853718747E-12));
#13612=CARTESIAN_POINT('',(-0.000258602011,-0.0104983385104078,-0.00434855707907396));
#13613=CARTESIAN_POINT('',(-0.000258602011,-0.00803511014973037,-0.00803508576177009));
#13614=CARTESIAN_POINT('',(-0.000258602011,-0.0043484665079003,-0.0104983454763083));
#13615=CARTESIAN_POINT('',(-0.000258602011,-0.00144971411419257,-0.0110749999993772));
#13616=CARTESIAN_POINT('',(-0.000258602011,-4.75766926220784E-12,-0.011075));
#13617=CARTESIAN_POINT('',(-0.00025860238623378,-9.94454622315446E-13,-0.0110749999999153));
#13618=CARTESIAN_POINT('',(-0.000258602071199268,-6.4246432521501E-12,0.0110749999882117));
#13619=CARTESIAN_POINT('',(-0.000258602011467561,4.51272795225522E-14,-3.71516306442422E-19));
#13620=CARTESIAN_POINT('',(0.0045,-2.22911966663019E-18,1.73472347597681E-20));
#13621=CARTESIAN_POINT('',(0.00450000000033692,3.48751202232752E-13,1.08129136841049E-19));
#13622=CARTESIAN_POINT('',(0.00450000000033692,6.37547546112859E-19,0.00779999999980785));
#13623=CARTESIAN_POINT('',(0.00450000000036139,-1.95000042881955E-12,-0.00779999999974705));
#13624=CARTESIAN_POINT('',(0.00450000000033692,-3.48751060863252E-13,-4.06296004640648E-19));
#13625=CARTESIAN_POINT('',(-1.1543990834159E-13,-4.73314002437894E-14,3.54060453998605E-19));
#13626=CARTESIAN_POINT('',(-0.0010062306454784,7.00818953022586E-18,-0.00885000006260538));
#13627=CARTESIAN_POINT('',(-0.00132239692205273,3.80617846662212E-15,-0.00920348474991875));
#13628=CARTESIAN_POINT('',(-0.00153614703263649,9.26191304452231E-15,-0.0102661649538024));
#13629=CARTESIAN_POINT('',(-0.000724069398158462,4.2080152504004E-15,-0.0109841539795411));
#13630=CARTESIAN_POINT('',(-0.000258602372466113,5.89741576151065E-17,-0.0110749999293739));
#13631=CARTESIAN_POINT('',(-0.00100623071506661,-7.94670107870803E-13,-0.0088500000003638));
#13632=CARTESIAN_POINT('',(-0.000258602011467561,1.98785142045412E-17,0.0110749999998306));
#13633=CARTESIAN_POINT('',(-0.000724069122077457,4.17825833481557E-15,0.0109841541650723));
#13634=CARTESIAN_POINT('',(-0.00153614703309098,9.25202015462542E-15,0.0102661651868448));
#13635=CARTESIAN_POINT('',(-0.00132239696292048,3.81144573458941E-15,0.0092034847956103));
#13636=CARTESIAN_POINT('',(-0.0010062306454784,1.90012882174815E-17,0.00885000006260538));
#13637=CARTESIAN_POINT('',(-0.00100623071506661,-6.59462196535367E-12,0.0088500000003638));
#13638=CARTESIAN_POINT('',(-0.00100623059013322,-6.59462086751533E-12,0.00885000000072759));
#13639=CARTESIAN_POINT('',(-0.00100623059014309,-0.00115846229739644,0.00884999999986943));
#13640=CARTESIAN_POINT('',(-0.00100623059016283,-0.00347484682895264,0.0083891970618622));
#13641=CARTESIAN_POINT('',(-0.00100623059018793,-0.0064208329443351,0.00642081345110636));
#13642=CARTESIAN_POINT('',(-0.00100623059020469,-0.00838919149809096,0.00347491919774606));
#13643=CARTESIAN_POINT('',(-0.00100623059021058,-0.00908040425267338,-2.97546799044951E-12));
#13644=CARTESIAN_POINT('',(-0.00100623059020469,-0.00838919149581363,-0.00347491920324402));
#13645=CARTESIAN_POINT('',(-0.00100623059018793,-0.00642083294012714,-0.00642081345531434));
#13646=CARTESIAN_POINT('',(-0.00100623059016283,-0.00347484682345468,-0.00838919706413948));
#13647=CARTESIAN_POINT('',(-0.00100623059014309,-0.00115846229159649,-0.00885000000062864));
#13648=CARTESIAN_POINT('',(-0.00100623059013322,-7.94669450589741E-13,-0.00885000000072759));
#13649=CARTESIAN_POINT('',(-1.1544007415132E-13,4.73304495273867E-14,-3.69660968558101E-19));
#13650=CARTESIAN_POINT('',(-0.00100623059013322,3.87578284472844E-14,-3.76880161186426E-19));
#13651=CARTESIAN_POINT('',(0.00420000000011192,-3.50891387635993E-13,-4.14898835309052E-19));
#13652=CARTESIAN_POINT('',(0.00420000000019215,8.38119770267861E-18,0.00749999999960454));
#13653=CARTESIAN_POINT('',(0.00435707963295547,-4.05846340527414E-15,0.00749999999964655));
#13654=CARTESIAN_POINT('',(0.00450000000032556,-1.62862306384024E-15,0.00764292036704453));
#13655=CARTESIAN_POINT('',(0.00450000000033692,-3.54563742746683E-19,0.00779999999980785));
#13656=CARTESIAN_POINT('',(0.00419999987517108,-1.5382740212674E-12,0.00749999999980227));
#13657=CARTESIAN_POINT('',(0.00450000000033692,-1.43886481780106E-17,-0.00779999999980785));
#13658=CARTESIAN_POINT('',(0.00450000000032556,-1.62909625669243E-15,-0.00764292036704453));
#13659=CARTESIAN_POINT('',(0.00435707963295547,-4.04642258766554E-15,-0.00749999999964655));
#13660=CARTESIAN_POINT('',(0.00420000000019215,3.31895800936513E-17,-0.00749999999960454));
#13661=CARTESIAN_POINT('',(0.00419999987509607,-4.29142485976802E-12,-0.00749999999980227));
#13662=CARTESIAN_POINT('',(0.00420000000019215,-4.29142066913366E-12,-0.00749999999960454));
#13663=CARTESIAN_POINT('',(0.00420000000020615,-0.00196349541225418,-0.00749999999857291));
#13664=CARTESIAN_POINT('',(0.00420000000023406,-0.0058748540154159,-0.00587708718402969));
#13665=CARTESIAN_POINT('',(0.00420000000025145,-0.00831257299276455,1.52571835373982E-12));
#13666=CARTESIAN_POINT('',(0.00420000000023406,-0.0058748540132585,0.00587708718618627));
#13667=CARTESIAN_POINT('',(0.00420000000020615,-0.00196349540950103,0.00749999999929369));
#13668=CARTESIAN_POINT('',(0.00420000000019215,-1.53826945716326E-12,0.00749999999960454));
#13669=CARTESIAN_POINT('',(0.00420000000011192,3.50891535870921E-13,1.16083160393565E-19));
#13670=CARTESIAN_POINT('',(0.00420000000011192,3.50891535870921E-13,1.16083160393565E-19));
#13671=CARTESIAN_POINT('',(-0.0206375,0.,0.));
#13672=CARTESIAN_POINT('',(-0.0045,0.,0.));
#13673=CARTESIAN_POINT('',(-0.0045,0.,-0.00885));
#13674=CARTESIAN_POINT('',(-0.0206375,0.,-2.47065262083525E-51));
#13675=CARTESIAN_POINT('',(-0.0042,-3.22189792023104E-12,-0.0075));
#13676=CARTESIAN_POINT('',(-0.0042,-0.0019634954110344,-0.00749999999915651));
#13677=CARTESIAN_POINT('',(-0.0042,-0.00587485401406066,-0.00587708718534322));
#13678=CARTESIAN_POINT('',(-0.0042,-0.00831257299263083,-9.5852737806285E-13));
#13679=CARTESIAN_POINT('',(-0.0042,-0.00587485401541604,0.00587708718398836));
#13680=CARTESIAN_POINT('',(-0.0042,-0.00196349541276405,0.00749999999870368));
#13681=CARTESIAN_POINT('',(-0.0042,-4.95155158286816E-12,0.0075));
#13682=CARTESIAN_POINT('',(-0.00419999962509607,-1.53827397134479E-12,0.00749999999980227));
#13683=CARTESIAN_POINT('',(-0.00420000000009607,-3.48594912388589E-12,-0.00749999999980227));
#13684=CARTESIAN_POINT('',(-0.00420000000011191,3.50891751372691E-13,2.79083595183788E-19));
#13685=CARTESIAN_POINT('',(-0.0045,-4.07660016854549E-19,-7.28583859910259E-19));
#13686=CARTESIAN_POINT('',(-0.00450000000033692,3.48751417212871E-13,2.87745340681233E-19));
#13687=CARTESIAN_POINT('',(-0.00450000000033692,-2.42388042693057E-19,-0.00779999999980785));
#13688=CARTESIAN_POINT('',(-0.00450000000036139,-1.9500002825196E-12,0.00779999999974705));
#13689=CARTESIAN_POINT('',(-0.00450000000033692,-3.48750946764454E-13,-1.41700427235676E-19));
#13690=CARTESIAN_POINT('',(-0.00420000000011191,-3.50891287789699E-13,-1.29656749332468E-19));
#13691=CARTESIAN_POINT('',(-0.00450000000033692,-2.40464944123498E-19,0.00779999999980786));
#13692=CARTESIAN_POINT('',(-0.00450000000032556,-1.62850896504167E-15,0.00764292036704453));
#13693=CARTESIAN_POINT('',(-0.00435707963295547,-4.05835609638575E-15,0.00749999999964656));
#13694=CARTESIAN_POINT('',(-0.00420000000019214,8.48104399744249E-18,0.00749999999960455));
#13695=CARTESIAN_POINT('',(-0.00420000000019214,3.32894263884152E-17,-0.00749999999960455));
#13696=CARTESIAN_POINT('',(-0.00435707963295547,-4.04631527877715E-15,-0.00749999999964656));
#13697=CARTESIAN_POINT('',(-0.00450000000032556,-1.62898215789386E-15,-0.00764292036704453));
#13698=CARTESIAN_POINT('',(-0.00450000000033692,-1.42745493793874E-17,-0.00779999999980786));
#13699=CARTESIAN_POINT('',(-0.00420000000011191,3.50891751372691E-13,2.79083595183788E-19));
#13700=CARTESIAN_POINT('',(0.0175000000000004,0.0150000000000004,1.10617214860196E-34));
#13701=CARTESIAN_POINT('',(0.035,0.,0.));
#13702=CARTESIAN_POINT('',(0.039,0.,0.));
#13703=CARTESIAN_POINT('',(0.039,0.,-0.016));
#13704=CARTESIAN_POINT('',(0.0385,0.,0.));
#13705=CARTESIAN_POINT('',(0.0385,0.,-0.016));
#13706=CARTESIAN_POINT('',(0.039,2.27769192395755E-17,1.36175792864179E-18));
#13707=CARTESIAN_POINT('',(0.039,0.,0.));
#13708=CARTESIAN_POINT('',(0.039,0.,0.01635));
#13709=CARTESIAN_POINT('',(0.0385,2.27769192395755E-17,-1.36175792864179E-18));
#13710=CARTESIAN_POINT('',(0.0385,0.,0.));
#13711=CARTESIAN_POINT('',(0.0385,0.,0.01635));
#13712=CARTESIAN_POINT('',(-2.34971638048196E-35,0.,0.));
#13713=CARTESIAN_POINT('',(0.0395,0.,0.));
#13714=CARTESIAN_POINT('',(0.0395,0.,0.01635));
#13715=CARTESIAN_POINT('',(-1.59983634253706E-35,0.,0.));
#13716=CARTESIAN_POINT('',(0.038,0.,0.));
#13717=CARTESIAN_POINT('',(0.038,0.,0.01635));
#13718=CARTESIAN_POINT('',(0.0395,2.27769192395755E-17,-1.36175792864179E-18));
#13719=CARTESIAN_POINT('',(0.0395,0.,0.));
#13720=CARTESIAN_POINT('',(0.0395,0.,-0.016));
#13721=CARTESIAN_POINT('',(0.038,2.27769192395755E-17,1.36175792864179E-18));
#13722=CARTESIAN_POINT('',(0.038,0.,0.));
#13723=CARTESIAN_POINT('',(0.038,0.,-0.016));
#13724=CARTESIAN_POINT('',(0.035,0.,0.));
#13725=CARTESIAN_POINT('',(0.04,0.,0.));
#13726=CARTESIAN_POINT('',(0.04,0.,-0.016));
#13727=CARTESIAN_POINT('',(0.035,0.,0.));
#13728=CARTESIAN_POINT('',(0.0375,0.,0.));
#13729=CARTESIAN_POINT('',(0.0375,0.,-0.016));
#13730=CARTESIAN_POINT('',(0.04,2.27769192395755E-17,1.36175792864179E-18));
#13731=CARTESIAN_POINT('',(0.04,0.,0.));
#13732=CARTESIAN_POINT('',(0.04,0.,0.01635));
#13733=CARTESIAN_POINT('',(0.0375,2.27769192395755E-17,-1.36175792864179E-18));
#13734=CARTESIAN_POINT('',(0.0375,0.,0.));
#13735=CARTESIAN_POINT('',(0.0375,0.,0.01635));
#13736=CARTESIAN_POINT('',(3.30786158221799E-36,0.,0.));
#13737=CARTESIAN_POINT('',(0.0405,0.,0.));
#13738=CARTESIAN_POINT('',(0.0405,0.,0.01635));
#13739=CARTESIAN_POINT('',(-1.05348069718484E-35,0.,0.));
#13740=CARTESIAN_POINT('',(0.037,0.,0.));
#13741=CARTESIAN_POINT('',(0.037,0.,0.01635));
#13742=CARTESIAN_POINT('',(0.0405,2.27769192395755E-17,-1.36175792864179E-18));
#13743=CARTESIAN_POINT('',(0.0405,0.,0.));
#13744=CARTESIAN_POINT('',(0.0405,0.,-0.016));
#13745=CARTESIAN_POINT('',(0.037,2.27769192395755E-17,1.36175792864179E-18));
#13746=CARTESIAN_POINT('',(0.037,0.,0.));
#13747=CARTESIAN_POINT('',(0.037,0.,-0.016));
#13748=CARTESIAN_POINT('',(0.035,0.,0.));
#13749=CARTESIAN_POINT('',(0.041,0.,0.));
#13750=CARTESIAN_POINT('',(0.041,0.,-0.016));
#13751=CARTESIAN_POINT('',(0.035,0.,0.));
#13752=CARTESIAN_POINT('',(0.0365,0.,0.));
#13753=CARTESIAN_POINT('',(0.0365,0.,-0.016));
#13754=CARTESIAN_POINT('',(0.041,2.27769192395755E-17,1.36175792864179E-18));
#13755=CARTESIAN_POINT('',(0.041,0.,0.));
#13756=CARTESIAN_POINT('',(0.041,0.,0.01635));
#13757=CARTESIAN_POINT('',(0.0365,2.27769192395755E-17,-1.36175792864179E-18));
#13758=CARTESIAN_POINT('',(0.0365,0.,0.));
#13759=CARTESIAN_POINT('',(0.0365,0.,0.01635));
#13760=CARTESIAN_POINT('',(-4.19093679253767E-36,0.,0.));
#13761=CARTESIAN_POINT('',(0.0415,0.,0.));
#13762=CARTESIAN_POINT('',(0.0415,0.,0.01635));
#13763=CARTESIAN_POINT('',(-3.03600664661662E-36,0.,0.));
#13764=CARTESIAN_POINT('',(0.036,0.,0.));
#13765=CARTESIAN_POINT('',(0.036,0.,0.01635));
#13766=CARTESIAN_POINT('',(0.0415,2.27769192395755E-17,-1.36175792864179E-18));
#13767=CARTESIAN_POINT('',(0.0415,0.,0.));
#13768=CARTESIAN_POINT('',(0.0415,0.,-0.016));
#13769=CARTESIAN_POINT('',(0.036,2.27769192395755E-17,1.36175792864179E-18));
#13770=CARTESIAN_POINT('',(0.036,0.,0.));
#13771=CARTESIAN_POINT('',(0.036,0.,-0.016));
#13772=CARTESIAN_POINT('',(0.035,0.,0.));
#13773=CARTESIAN_POINT('',(0.042,0.,0.));
#13774=CARTESIAN_POINT('',(0.042,0.,-0.016));
#13775=CARTESIAN_POINT('',(0.035,0.,0.));
#13776=CARTESIAN_POINT('',(0.035,0.,0.));
#13777=CARTESIAN_POINT('',(0.035,0.,-0.016));
#13778=CARTESIAN_POINT('',(0.042,-3.07046055247895E-18,0.));
#13779=CARTESIAN_POINT('',(0.042,0.,0.));
#13780=CARTESIAN_POINT('',(0.042,0.,0.0175));
#13781=CARTESIAN_POINT('',(0.035,-3.98986399474666E-19,1.35308431126191E-18));
#13782=CARTESIAN_POINT('',(0.035,0.,0.));
#13783=CARTESIAN_POINT('',(0.035,0.,-0.0125));
#13784=CARTESIAN_POINT('',(0.046000012,0.,0.));
#13785=CARTESIAN_POINT('',(0.046,0.,0.));
#13786=CARTESIAN_POINT('',(0.046,0.,0.0175));
#13787=CARTESIAN_POINT('',(0.028,0.,0.));
#13788=CARTESIAN_POINT('',(0.028,0.,0.));
#13789=CARTESIAN_POINT('',(0.028,0.,-0.0125));
#13790=CARTESIAN_POINT('',(0.046,-5.46437894932694E-19,-1.3010426069826E-18));
#13791=CARTESIAN_POINT('',(0.046,0.,0.));
#13792=CARTESIAN_POINT('',(0.046,0.,0.0185));
#13793=CARTESIAN_POINT('',(0.028,-5.20417042793042E-19,1.39645239816133E-18));
#13794=CARTESIAN_POINT('',(0.028,0.,0.));
#13795=CARTESIAN_POINT('',(0.028,0.,-0.0115));
#13796=CARTESIAN_POINT('',(-0.087860759494,0.,0.));
#13797=CARTESIAN_POINT('',(0.042,0.,0.));
#13798=CARTESIAN_POINT('',(0.042,0.,0.0185));
#13799=CARTESIAN_POINT('',(0.028,0.,0.));
#13800=CARTESIAN_POINT('',(0.0259999999999953,0.,0.));
#13801=CARTESIAN_POINT('',(0.0259999999999953,0.,0.0114999999999814));
#13802=CARTESIAN_POINT('',(0.042,-2.55351295663786E-17,-2.63677968348474E-18));
#13803=CARTESIAN_POINT('',(0.0419999999998646,-1.37313705098871E-13,-8.69099870562485E-19));
#13804=CARTESIAN_POINT('',(0.0419999999999067,0.0329999999999944,-8.69099870562485E-19));
#13805=CARTESIAN_POINT('',(0.042,0.027720932313,-0.010089594228));
#13806=CARTESIAN_POINT('',(0.042,0.027720932313,-0.011389594228));
#13807=CARTESIAN_POINT('',(0.042,0.022598311072,-0.018962234486));
#13808=CARTESIAN_POINT('',(0.042,0.022598311072,-0.020262234486));
#13809=CARTESIAN_POINT('',(0.042,0.01475,-0.025547749412));
#13810=CARTESIAN_POINT('',(0.042,0.01475,-0.026847749412));
#13811=CARTESIAN_POINT('',(0.042,0.005122621241,-0.029051828714));
#13812=CARTESIAN_POINT('',(0.042,0.005122621241,-0.030351828714));
#13813=CARTESIAN_POINT('',(0.042,-0.005122621241,-0.029051828714));
#13814=CARTESIAN_POINT('',(0.042,-0.005122621241,-0.030351828714));
#13815=CARTESIAN_POINT('',(0.042,-0.01475,-0.025547749412));
#13816=CARTESIAN_POINT('',(0.042,-0.01475,-0.026847749412));
#13817=CARTESIAN_POINT('',(0.042,-0.022598311072,-0.018962234486));
#13818=CARTESIAN_POINT('',(0.042,-0.022598311072,-0.020262234486));
#13819=CARTESIAN_POINT('',(0.042,-0.027720932313,-0.010089594228));
#13820=CARTESIAN_POINT('',(0.042,-0.027720932313,-0.011389594228));
#13821=CARTESIAN_POINT('',(0.042,-0.0295,0.));
#13822=CARTESIAN_POINT('',(0.042,-0.0295,-0.0013));
#13823=CARTESIAN_POINT('',(0.042,-0.027720932313,0.010089594228));
#13824=CARTESIAN_POINT('',(0.042,-0.027720932313,0.008789594228));
#13825=CARTESIAN_POINT('',(0.042,-0.022598311072,0.018962234486));
#13826=CARTESIAN_POINT('',(0.042,-0.022598311072,0.017662234486));
#13827=CARTESIAN_POINT('',(0.042,-0.01475,0.025547749412));
#13828=CARTESIAN_POINT('',(0.042,-0.01475,0.024247749412));
#13829=CARTESIAN_POINT('',(0.042,-0.005122621241,0.029051828714));
#13830=CARTESIAN_POINT('',(0.042,-0.005122621241,0.027751828714));
#13831=CARTESIAN_POINT('',(0.042,0.005122621241,0.029051828714));
#13832=CARTESIAN_POINT('',(0.042,0.005122621241,0.027751828714));
#13833=CARTESIAN_POINT('',(0.042,0.01475,0.025547749412));
#13834=CARTESIAN_POINT('',(0.042,0.01475,0.024247749412));
#13835=CARTESIAN_POINT('',(0.042,0.022598311072,0.018962234486));
#13836=CARTESIAN_POINT('',(0.042,0.022598311072,0.017662234486));
#13837=CARTESIAN_POINT('',(0.042,0.027720932313,0.010089594228));
#13838=CARTESIAN_POINT('',(0.042,0.027720932313,0.008789594228));
#13839=CARTESIAN_POINT('',(0.042,0.0295,0.));
#13840=CARTESIAN_POINT('',(0.042,0.0295,-0.0013));
#13841=CARTESIAN_POINT('',(0.071999999999921,0.,0.));
#13842=CARTESIAN_POINT('',(0.024,0.,0.));
#13843=CARTESIAN_POINT('',(0.024,0.,-0.012));
#13844=CARTESIAN_POINT('',(-0.046,0.0295,0.));
#13845=CARTESIAN_POINT('',(0.039,0.0295,0.));
#13846=CARTESIAN_POINT('',(0.039,0.0295,-0.0013));
#13847=CARTESIAN_POINT('',(-0.046,0.027720932313,0.010089594228));
#13848=CARTESIAN_POINT('',(0.039,0.027720932313,0.010089594228));
#13849=CARTESIAN_POINT('',(0.039,0.027720932313,0.008789594228));
#13850=CARTESIAN_POINT('',(-0.046,0.022598311072,0.018962234486));
#13851=CARTESIAN_POINT('',(0.039,0.022598311072,0.018962234486));
#13852=CARTESIAN_POINT('',(0.039,0.022598311072,0.017662234486));
#13853=CARTESIAN_POINT('',(-0.046,0.01475,0.025547749412));
#13854=CARTESIAN_POINT('',(0.039,0.01475,0.025547749412));
#13855=CARTESIAN_POINT('',(0.039,0.01475,0.024247749412));
#13856=CARTESIAN_POINT('',(-0.046,0.005122621241,0.029051828714));
#13857=CARTESIAN_POINT('',(0.039,0.005122621241,0.029051828714));
#13858=CARTESIAN_POINT('',(0.039,0.005122621241,0.027751828714));
#13859=CARTESIAN_POINT('',(-0.046,-0.005122621241,0.029051828714));
#13860=CARTESIAN_POINT('',(0.039,-0.005122621241,0.029051828714));
#13861=CARTESIAN_POINT('',(0.039,-0.005122621241,0.027751828714));
#13862=CARTESIAN_POINT('',(-0.046,-0.01475,0.025547749412));
#13863=CARTESIAN_POINT('',(0.039,-0.01475,0.025547749412));
#13864=CARTESIAN_POINT('',(0.039,-0.01475,0.024247749412));
#13865=CARTESIAN_POINT('',(-0.046,-0.022598311072,0.018962234486));
#13866=CARTESIAN_POINT('',(0.039,-0.022598311072,0.018962234486));
#13867=CARTESIAN_POINT('',(0.039,-0.022598311072,0.017662234486));
#13868=CARTESIAN_POINT('',(-0.046,-0.027720932313,0.010089594228));
#13869=CARTESIAN_POINT('',(0.039,-0.027720932313,0.010089594228));
#13870=CARTESIAN_POINT('',(0.039,-0.027720932313,0.008789594228));
#13871=CARTESIAN_POINT('',(-0.046,-0.0295,0.));
#13872=CARTESIAN_POINT('',(0.039,-0.0295,0.));
#13873=CARTESIAN_POINT('',(0.039,-0.0295,-0.0013));
#13874=CARTESIAN_POINT('',(-0.046,-0.027720932313,-0.010089594228));
#13875=CARTESIAN_POINT('',(0.039,-0.027720932313,-0.010089594228));
#13876=CARTESIAN_POINT('',(0.039,-0.027720932313,-0.011389594228));
#13877=CARTESIAN_POINT('',(-0.046,-0.022598311072,-0.018962234486));
#13878=CARTESIAN_POINT('',(0.039,-0.022598311072,-0.018962234486));
#13879=CARTESIAN_POINT('',(0.039,-0.022598311072,-0.020262234486));
#13880=CARTESIAN_POINT('',(-0.046,-0.01475,-0.025547749412));
#13881=CARTESIAN_POINT('',(0.039,-0.01475,-0.025547749412));
#13882=CARTESIAN_POINT('',(0.039,-0.01475,-0.026847749412));
#13883=CARTESIAN_POINT('',(-0.046,-0.005122621241,-0.029051828714));
#13884=CARTESIAN_POINT('',(0.039,-0.005122621241,-0.029051828714));
#13885=CARTESIAN_POINT('',(0.039,-0.005122621241,-0.030351828714));
#13886=CARTESIAN_POINT('',(-0.046,0.005122621241,-0.029051828714));
#13887=CARTESIAN_POINT('',(0.039,0.005122621241,-0.029051828714));
#13888=CARTESIAN_POINT('',(0.039,0.005122621241,-0.030351828714));
#13889=CARTESIAN_POINT('',(-0.046,0.01475,-0.025547749412));
#13890=CARTESIAN_POINT('',(0.039,0.01475,-0.025547749412));
#13891=CARTESIAN_POINT('',(0.039,0.01475,-0.026847749412));
#13892=CARTESIAN_POINT('',(-0.046,0.022598311072,-0.018962234486));
#13893=CARTESIAN_POINT('',(0.039,0.022598311072,-0.018962234486));
#13894=CARTESIAN_POINT('',(0.039,0.022598311072,-0.020262234486));
#13895=CARTESIAN_POINT('',(-0.046,0.027720932313,-0.010089594228));
#13896=CARTESIAN_POINT('',(0.039,0.027720932313,-0.010089594228));
#13897=CARTESIAN_POINT('',(0.039,0.027720932313,-0.011389594228));
#13898=CARTESIAN_POINT('',(0.0410000000000154,-1.36037053452222E-13,-7.67814047972691E-19));
#13899=CARTESIAN_POINT('',(0.0410000000001318,1.36039880532457E-13,1.32586349256442E-18));
#13900=CARTESIAN_POINT('',(0.0409999998753159,-6.97350952530812E-12,-0.0339999999999195));
#13901=CARTESIAN_POINT('',(0.0409999998750659,-1.9454455441122E-11,0.0339999999999195));
#13902=CARTESIAN_POINT('',(0.0410000000001318,-1.94544627178456E-11,0.0339999999998389));
#13903=CARTESIAN_POINT('',(0.0410000000001261,-0.00445058961092909,0.0339999999973102));
#13904=CARTESIAN_POINT('',(0.0410000000001147,-0.01334969402564,0.0322296836269298));
#13905=CARTESIAN_POINT('',(0.0410000000001003,-0.0246676067857547,0.02466753190434));
#13906=CARTESIAN_POINT('',(0.0410000000000906,-0.0322296622477484,0.0133499720628637));
#13907=CARTESIAN_POINT('',(0.0410000000000872,-0.0348851688773134,-6.40291906310467E-12));
#13908=CARTESIAN_POINT('',(0.0410000000000906,-0.0322296622428478,-0.0133499720746949));
#13909=CARTESIAN_POINT('',(0.0410000000001003,-0.0246676067766995,-0.0246675319133952));
#13910=CARTESIAN_POINT('',(0.0410000000001147,-0.0133496940138089,-0.0322296836318303));
#13911=CARTESIAN_POINT('',(0.0410000000001261,-0.00445058959844814,-0.0339999999989439));
#13912=CARTESIAN_POINT('',(0.0410000000001318,-6.97351966199401E-12,-0.0339999999998389));
#13913=CARTESIAN_POINT('',(0.028,0.,0.));
#13914=CARTESIAN_POINT('',(-0.0320000000000083,0.,0.));
#13915=CARTESIAN_POINT('',(-0.0319999999981381,-0.0119999999536082,-4.92248153054964E-12));
#13916=CARTESIAN_POINT('',(-0.0320000001856381,0.0119999999536082,3.42248023884155E-12));
#13917=CARTESIAN_POINT('',(-0.032,-0.012,-1.9225239339229E-12));
#13918=CARTESIAN_POINT('',(-0.032,-0.0120000000002517,0.00157079632480987));
#13919=CARTESIAN_POINT('',(-0.032,-0.0113751824597898,0.0047116567075861));
#13920=CARTESIAN_POINT('',(-0.032,-0.00870618773601581,0.00870621415482392));
#13921=CARTESIAN_POINT('',(-0.032,-0.00471175485132592,0.0113751749088022));
#13922=CARTESIAN_POINT('',(-0.032,-2.74207991250776E-12,0.0123124125450742));
#13923=CARTESIAN_POINT('',(-0.032,0.00471175484625923,0.0113751749109008));
#13924=CARTESIAN_POINT('',(-0.032,0.0087061877321379,0.00870621415870182));
#13925=CARTESIAN_POINT('',(-0.032,0.0113751824576911,0.00471165671265278));
#13926=CARTESIAN_POINT('',(-0.032,0.011999999999552,0.00157079633015488));
#13927=CARTESIAN_POINT('',(-0.032,0.012,3.42248023051021E-12));
#13928=CARTESIAN_POINT('',(0.039,-2.55351295663786E-17,2.63677968348474E-18));
#13929=CARTESIAN_POINT('',(0.0390000000001354,-1.37315511707168E-13,3.70144955568662E-19));
#13930=CARTESIAN_POINT('',(0.0390000000000933,0.0329999999999944,3.70144955568662E-19));
#13931=CARTESIAN_POINT('',(0.039,0.,0.));
#13932=CARTESIAN_POINT('',(0.039,0.,0.0195));
#13933=CARTESIAN_POINT('',(-0.087860759494,0.,0.));
#13934=CARTESIAN_POINT('',(0.04,-2.24470338423357E-11,-0.034));
#13935=CARTESIAN_POINT('',(0.04,-0.0044505896134887,-0.0339999999970617));
#13936=CARTESIAN_POINT('',(0.04,-0.0133496940271719,-0.0322296836262199));
#13937=CARTESIAN_POINT('',(0.04,-0.0246676067858995,-0.0246675319040342));
#13938=CARTESIAN_POINT('',(0.04,-0.03222966224722,-0.0133499720637649));
#13939=CARTESIAN_POINT('',(0.04,-0.0348851688771597,4.02261648685935E-12));
#13940=CARTESIAN_POINT('',(0.04,-0.0322296622441412,0.0133499720711977));
#13941=CARTESIAN_POINT('',(0.04,-0.0246676067802106,0.0246675319097231));
#13942=CARTESIAN_POINT('',(0.04,-0.0133496940197391,0.0322296836292986));
#13943=CARTESIAN_POINT('',(0.04,-0.0044505896056476,0.0339999999980881));
#13944=CARTESIAN_POINT('',(0.04,-1.46059372383807E-11,0.034));
#13945=CARTESIAN_POINT('',(0.04,-1.15529693224835E-11,0.034));
#13946=CARTESIAN_POINT('',(0.0400000003749341,-6.97351034698232E-12,-0.0339999999999195));
#13947=CARTESIAN_POINT('',(0.04,0.,0.));
#13948=CARTESIAN_POINT('',(-0.0800000000001418,0.,0.));
#13949=CARTESIAN_POINT('',(-0.034,0.,0.));
#13950=CARTESIAN_POINT('',(-0.0340000000018702,-0.0115000000464252,-4.71737817072462E-12));
#13951=CARTESIAN_POINT('',(-0.0340000001875042,0.0115000000000167,3.27988199461071E-12));
#13952=CARTESIAN_POINT('',(-0.0340000000000083,-0.0115000000000334,-1.84241877001479E-12));
#13953=CARTESIAN_POINT('',(-0.0340000000000083,-0.0115000000002745,0.00150534647794716));
#13954=CARTESIAN_POINT('',(-0.0340000000000083,-0.0109012165239968,0.00451533767811645));
#13955=CARTESIAN_POINT('',(-0.0340000000000083,-0.00834342991370603,0.00834345523173046));
#13956=CARTESIAN_POINT('',(-0.0340000000000083,-0.00451543173253378,0.0109012092876337));
#13957=CARTESIAN_POINT('',(-0.0340000000000083,-2.62782831866655E-12,0.0117993953557304));
#13958=CARTESIAN_POINT('',(-0.0340000000000083,0.00451543172767821,0.0109012092896449));
#13959=CARTESIAN_POINT('',(-0.0340000000000083,0.00834342990998969,0.0083434552354468));
#13960=CARTESIAN_POINT('',(-0.0340000000000083,0.0109012165219856,0.00451533768297201));
#13961=CARTESIAN_POINT('',(-0.0340000000000083,0.011499999999604,0.00150534648306946));
#13962=CARTESIAN_POINT('',(-0.0340000000000083,0.0115000000000334,3.27987688758181E-12));
#13963=CARTESIAN_POINT('',(-0.087860759494,0.,0.));
#13964=CARTESIAN_POINT('',(0.034,4.875E-12,0.0195));
#13965=CARTESIAN_POINT('',(0.034,0.00255254403584375,0.0194999999993619));
#13966=CARTESIAN_POINT('',(0.034,0.00765644215749575,0.0184846714939946));
#13967=CARTESIAN_POINT('',(0.034,0.014147598007525,0.0141475550651059));
#13968=CARTESIAN_POINT('',(0.034,0.0184846592300561,0.0076566016255824));
#13969=CARTESIAN_POINT('',(0.034,0.0200076703857572,-4.10364388936103E-12));
#13970=CARTESIAN_POINT('',(0.034,0.0184846592269153,-0.00765660163316493));
#13971=CARTESIAN_POINT('',(0.034,0.0141475980017216,-0.0141475550709093));
#13972=CARTESIAN_POINT('',(0.034,0.0076564421499132,-0.0184846714971353));
#13973=CARTESIAN_POINT('',(0.034,0.00255254402784472,-0.0195000000004089));
#13974=CARTESIAN_POINT('',(0.034,-3.12403330873861E-12,-0.0195));
#13975=CARTESIAN_POINT('',(0.0340000000083513,-5.99926878926874E-12,-0.0194999999687883));
#13976=CARTESIAN_POINT('',(0.0340000000083513,-2.8752398984365E-12,0.0194999999687883));
#13977=CARTESIAN_POINT('',(0.034,-1.28740341154572E-11,-0.0195));
#13978=CARTESIAN_POINT('',(0.034,-0.00255254404303028,-0.0194999999983148));
#13979=CARTESIAN_POINT('',(0.034,-0.00765644216264269,-0.0184846714915085));
#13980=CARTESIAN_POINT('',(0.034,-0.01414759800956,-0.0141475550626079));
#13981=CARTESIAN_POINT('',(0.034,-0.0184846592300232,-0.00765660162480633));
#13982=CARTESIAN_POINT('',(0.034,-0.0200076703854298,2.30708918532461E-12));
#13983=CARTESIAN_POINT('',(0.034,-0.0184846592282575,0.00765660162906927));
#13984=CARTESIAN_POINT('',(0.034,-0.0141475980062973,0.0141475550658706));
#13985=CARTESIAN_POINT('',(0.034,-0.00765644215837976,0.0184846714932742));
#13986=CARTESIAN_POINT('',(0.034,-0.00255254403853318,0.0194999999989035));
#13987=CARTESIAN_POINT('',(0.034,-8.37693459260071E-12,0.0195));
#13988=CARTESIAN_POINT('',(0.0399999999999847,-1.36038696801256E-13,4.00781722114515E-19));
#13989=CARTESIAN_POINT('',(0.028,0.,0.));
#13990=CARTESIAN_POINT('',(-0.036,0.,0.));
#13991=CARTESIAN_POINT('',(-0.036,0.,-0.0115));
#13992=CARTESIAN_POINT('',(0.000225009254313235,0.,0.));
#13993=CARTESIAN_POINT('',(0.0284641016149117,-7.00391101341243E-12,-0.016303847577153));
#13994=CARTESIAN_POINT('',(0.0284641016149117,-0.00213416866341332,-0.0163038475762362));
#13995=CARTESIAN_POINT('',(0.0284641016149117,-0.00640151107325889,-0.015454936745714));
#13996=CARTESIAN_POINT('',(0.0284641016149117,-0.0118287323830679,-0.011828696481542));
#13997=CARTESIAN_POINT('',(0.0284641016149117,-0.0154549264905978,-0.00640164440683067));
#13998=CARTESIAN_POINT('',(0.0284641016149117,-0.0167283081198615,-2.97447703265889E-12));
#13999=CARTESIAN_POINT('',(0.0284641016149117,-0.0154549264928743,0.00640164440133462));
#14000=CARTESIAN_POINT('',(0.0284641016149117,-0.0118287323872744,0.0118286964773355));
#14001=CARTESIAN_POINT('',(0.0284641016149117,-0.00640151107875499,0.0154549367434375));
#14002=CARTESIAN_POINT('',(0.0284641016149117,-0.0021341686692113,0.0163038475754773));
#14003=CARTESIAN_POINT('',(0.0284641016149117,-1.28018861790704E-11,0.016303847577153));
#14004=CARTESIAN_POINT('',(0.0284641017231648,-1.28018825845269E-11,0.016303847639653));
#14005=CARTESIAN_POINT('',(0.028464101723209,-5.53993719574163E-12,-0.0163038476395765));
#14006=CARTESIAN_POINT('',(0.0284641016149116,0.,0.));
#14007=CARTESIAN_POINT('',(-0.036,-5.20417042793042E-19,-1.39645239816133E-18));
#14008=CARTESIAN_POINT('',(-0.036,0.,0.));
#14009=CARTESIAN_POINT('',(-0.036,0.,-0.0125));
#14010=CARTESIAN_POINT('',(0.0274641016153175,3.0328372677955E-13,-6.78218228121713E-19));
#14011=CARTESIAN_POINT('',(0.0274641016157182,5.28701310234456E-17,-0.0160358983846333));
#14012=CARTESIAN_POINT('',(0.0278131674658368,3.8206405763144E-16,-0.0160358983847033));
#14013=CARTESIAN_POINT('',(0.0281618017210979,-1.01223191233354E-15,-0.016129314652066));
#14014=CARTESIAN_POINT('',(0.0284641016147314,-5.8446799695983E-17,-0.0163038475774072));
#14015=CARTESIAN_POINT('',(0.0274641014903591,-3.28901507865897E-12,-0.0160358983848167));
#14016=CARTESIAN_POINT('',(0.027464101615,0.,2.55499381282536E-17));
#14017=CARTESIAN_POINT('',(0.0274641014903591,-7.17767932656037E-19,0.0160358983848167));
#14018=CARTESIAN_POINT('',(0.0284641016147314,-3.99727831696944E-17,0.0163038475774072));
#14019=CARTESIAN_POINT('',(0.0281618017210979,-1.02050365731269E-15,0.016129314652066));
#14020=CARTESIAN_POINT('',(0.0278131674658368,3.48011082928235E-16,0.0160358983847033));
#14021=CARTESIAN_POINT('',(0.0274641016157182,-7.29453163667589E-18,0.0160358983846333));
#14022=CARTESIAN_POINT('',(0.0274641016153175,-3.0328373862405E-13,1.10406601067048E-18));
#14023=CARTESIAN_POINT('',(0.0274641016157182,-3.28902052244081E-12,-0.0160358983846333));
#14024=CARTESIAN_POINT('',(0.0274641016158464,-0.00209909419313044,-0.0160358983842425));
#14025=CARTESIAN_POINT('',(0.0274641016161028,-0.00629630402099476,-0.0152009391671627));
#14026=CARTESIAN_POINT('',(0.0274641016164288,-0.0116343304626701,-0.0116342951504423));
#14027=CARTESIAN_POINT('',(0.0274641016166466,-0.0152009290811225,-0.00629643516240151));
#14028=CARTESIAN_POINT('',(0.0274641016167231,-0.0164533830371665,1.68734400876107E-12));
#14029=CARTESIAN_POINT('',(0.0274641016166466,-0.0152009290798311,0.00629643516551926));
#14030=CARTESIAN_POINT('',(0.0274641016164288,-0.0116343304602839,0.0116342951528286));
#14031=CARTESIAN_POINT('',(0.0274641016161028,-0.00629630401787699,0.0152009391684541));
#14032=CARTESIAN_POINT('',(0.0274641016158464,-0.00209909418984144,0.016035898384673));
#14033=CARTESIAN_POINT('',(0.0274641016157182,-1.92389594726442E-17,0.0160358983846333));
#14034=CARTESIAN_POINT('',(-0.046,0.,0.));
#14035=CARTESIAN_POINT('',(-0.0457000000001119,3.50888490739562E-13,-3.07178390214567E-19));
#14036=CARTESIAN_POINT('',(-0.045699999875,-5.80991519208953E-12,-0.0125));
#14037=CARTESIAN_POINT('',(-0.0457000000000961,-7.2512874463399E-12,0.0124999999998023));
#14038=CARTESIAN_POINT('',(-0.0457,-5.80992227401315E-12,-0.0125));
#14039=CARTESIAN_POINT('',(-0.0457,-0.00163624617896867,-0.0124999999992395));
#14040=CARTESIAN_POINT('',(-0.0457,-0.00490797574291331,-0.0118491483929665));
#14041=CARTESIAN_POINT('',(-0.0457,-0.00906897308119405,-0.00906894555480054));
#14042=CARTESIAN_POINT('',(-0.0457,-0.0118491405310354,-0.00490807796708854));
#14043=CARTESIAN_POINT('',(-0.0457,-0.0128254297342425,-1.25315075420625E-12));
#14044=CARTESIAN_POINT('',(-0.0457,-0.0118491405319946,0.00490807796477308));
#14045=CARTESIAN_POINT('',(-0.0457,-0.00906897308296621,0.00906894555302836));
#14046=CARTESIAN_POINT('',(-0.0457,-0.0049079757452288,0.0118491483920074));
#14047=CARTESIAN_POINT('',(-0.0457,-0.00163624618141133,0.0124999999989197));
#14048=CARTESIAN_POINT('',(-0.0457,-8.25258597144694E-12,0.0125));
#14049=CARTESIAN_POINT('',(-0.087860759494,0.,5.07655879918927E-49));
#14050=CARTESIAN_POINT('',(-0.024585786438,-7.45336965029581E-12,0.016035898385));
#14051=CARTESIAN_POINT('',(-0.024585786438,0.000957895816119835,0.0160358983854452));
#14052=CARTESIAN_POINT('',(-0.024585786438,0.00191577520026407,0.015949840337913));
#14053=CARTESIAN_POINT('',(-0.024585786438,0.00285833127640244,0.0157790994460516));
#14054=CARTESIAN_POINT('',(-0.0245857915218893,0.00285875682645188,0.0157810768606755));
#14055=CARTESIAN_POINT('',(-0.024585786063,-7.45336965029578E-12,0.016035898385));
#14056=CARTESIAN_POINT('',(-0.024585786438,-0.00285833128348905,0.0157790994447679));
#14057=CARTESIAN_POINT('',(-0.024585786438,-0.00191577520995451,0.0159498403365949));
#14058=CARTESIAN_POINT('',(-0.024585786438,-0.00095789582845831,0.0160358983845548));
#14059=CARTESIAN_POINT('',(-0.024585786438,-7.45337161412695E-12,0.016035898385));
#14060=CARTESIAN_POINT('',(-0.0245857915247488,-0.00285875721875978,0.0157810777875231));
#14061=CARTESIAN_POINT('',(-0.0244999999986063,-0.0038308953218821,0.0155715855983528));
#14062=CARTESIAN_POINT('',(-0.0244999999986063,-0.00375675399330742,0.0155898257234191));
#14063=CARTESIAN_POINT('',(-0.0245092062752334,-0.00361121403183318,0.0156242768363253));
#14064=CARTESIAN_POINT('',(-0.0245230015373636,-0.00349407903633082,0.0156507180843297));
#14065=CARTESIAN_POINT('',(-0.0245385333070015,-0.00337456186848279,0.0156770044066975));
#14066=CARTESIAN_POINT('',(-0.024553360191519,-0.00326583388861101,0.0156998573759084));
#14067=CARTESIAN_POINT('',(-0.0245599200223058,-0.003216175379522,0.0157101139591801));
#14068=CARTESIAN_POINT('',(-0.0245794719072487,-0.00305592627035903,0.0157425438538854));
#14069=CARTESIAN_POINT('',(-0.024585786438,-0.0029347517273015,0.0157652561360282));
#14070=CARTESIAN_POINT('',(-0.024585786438,-0.00285833128348905,0.0157790994447679));
#14071=CARTESIAN_POINT('',(-0.0244999908748831,-0.00383146920545553,0.0155743307735512));
#14072=CARTESIAN_POINT('',(-0.0244999999986063,-0.0115699410488142,0.0111034454626035));
#14073=CARTESIAN_POINT('',(-0.0244999999986063,-0.00947974650797664,0.0132814565763153));
#14074=CARTESIAN_POINT('',(-0.0244999999986063,-0.0067622055462158,0.0148504295828361));
#14075=CARTESIAN_POINT('',(-0.0244999999986063,-0.0038308953218821,0.0155715855983528));
#14076=CARTESIAN_POINT('',(-0.024499990869348,-0.0115720326073917,0.0111053160311667));
#14077=CARTESIAN_POINT('',(-0.024585786438,-0.0122359353307441,0.01036493722103));
#14078=CARTESIAN_POINT('',(-0.024585786438,-0.0121857755381519,0.0104241514705014));
#14079=CARTESIAN_POINT('',(-0.0245794838708969,-0.0121055669343417,0.0105176812333229));
#14080=CARTESIAN_POINT('',(-0.0245599357702701,-0.0119973545564825,0.0106402513674701));
#14081=CARTESIAN_POINT('',(-0.0245533746790821,-0.0119636301855107,0.0106781433864587));
#14082=CARTESIAN_POINT('',(-0.0245385462358393,-0.0118894679802916,0.0107608868196226));
#14083=CARTESIAN_POINT('',(-0.0245230204403454,-0.0118069814705956,0.0108512096671411));
#14084=CARTESIAN_POINT('',(-0.0245092134847558,-0.011725477902448,0.0109394730212321));
#14085=CARTESIAN_POINT('',(-0.0244999999986063,-0.011622848024814,0.0110483156746966));
#14086=CARTESIAN_POINT('',(-0.0244999999986063,-0.0115699410488142,0.0111034454626035));
#14087=CARTESIAN_POINT('',(-0.0245857915218036,-0.0122374350471151,0.0103662944654208));
#14088=CARTESIAN_POINT('',(-0.024585786438,-0.0150942666086899,0.00541416222141845));
#14089=CARTESIAN_POINT('',(-0.024585786438,-0.0144474424338318,0.00721745812297648));
#14090=CARTESIAN_POINT('',(-0.024585786438,-0.0134742233042604,0.00890312310275038));
#14091=CARTESIAN_POINT('',(-0.024585786438,-0.0122359353307441,0.01036493722103));
#14092=CARTESIAN_POINT('',(-0.0245857915246625,-0.0150961928720038,0.00541478251987751));
#14093=CARTESIAN_POINT('',(-0.0244999999986063,-0.0154008363654399,0.00446814013421592));
#14094=CARTESIAN_POINT('',(-0.0244999999986063,-0.0153795621158588,0.00454146846026513));
#14095=CARTESIAN_POINT('',(-0.0245092062770903,-0.0153366276661337,0.00468473534680755));
#14096=CARTESIAN_POINT('',(-0.0245230015342683,-0.0153009589728398,0.00479939781420821));
#14097=CARTESIAN_POINT('',(-0.0245385333074752,-0.0152639650035507,0.0049160459052644));
#14098=CARTESIAN_POINT('',(-0.0245533601912854,-0.0152293922673203,0.00502163357681073));
#14099=CARTESIAN_POINT('',(-0.0245599200224393,-0.0152134454727527,0.00506976740392879));
#14100=CARTESIAN_POINT('',(-0.0245794719071485,-0.0151614060402287,0.00522476212260026));
#14101=CARTESIAN_POINT('',(-0.024585786438,-0.0151204881851425,0.00534105848907922));
#14102=CARTESIAN_POINT('',(-0.024585786438,-0.0150942666086899,0.00541416222141845));
#14103=CARTESIAN_POINT('',(-0.0244999908748826,-0.0154035006993891,0.00446901572194627));
#14104=CARTESIAN_POINT('',(-0.0244999999986063,-0.0154008363654352,-0.0044681401342319));
#14105=CARTESIAN_POINT('',(-0.0244999999986063,-0.0162419520486458,-0.00156897300599358));
#14106=CARTESIAN_POINT('',(-0.0244999999986063,-0.0162419520486474,0.00156897300597672));
#14107=CARTESIAN_POINT('',(-0.0244999999986063,-0.0154008363654399,0.00446814013421592));
#14108=CARTESIAN_POINT('',(-0.0244999908693475,-0.0154035021040441,-0.00446901619492932));
#14109=CARTESIAN_POINT('',(-0.024585786438,-0.0150942666084793,-0.00541416222200544));
#14110=CARTESIAN_POINT('',(-0.024585786438,-0.0151204677564812,-0.00534111544261991));
#14111=CARTESIAN_POINT('',(-0.024579483870953,-0.0151613626047746,-0.00522488787391248));
#14112=CARTESIAN_POINT('',(-0.0245599357701953,-0.0152134052666352,-0.00506988813579796));
#14113=CARTESIAN_POINT('',(-0.0245533746792129,-0.0152293585307658,-0.00502173596870886));
#14114=CARTESIAN_POINT('',(-0.0245385462343378,-0.0152639353408618,-0.00491613790530282));
#14115=CARTESIAN_POINT('',(-0.0245230204532045,-0.0153009139297729,-0.00479954118649679));
#14116=CARTESIAN_POINT('',(-0.0245092134770404,-0.0153366005165388,-0.00468482514492004));
#14117=CARTESIAN_POINT('',(-0.0244999999986063,-0.0153795460566674,-0.00454152381326889));
#14118=CARTESIAN_POINT('',(-0.0244999999986063,-0.0154008363654352,-0.0044681401342319));
#14119=CARTESIAN_POINT('',(-0.0245857915218038,-0.0150961918740712,-0.00541478239418764));
#14120=CARTESIAN_POINT('',(-0.024585786438,-0.0122359353199755,-0.0103649372337425));
#14121=CARTESIAN_POINT('',(-0.024585786438,-0.0134742232984657,-0.0089031231126705));
#14122=CARTESIAN_POINT('',(-0.024585786438,-0.0144474424317463,-0.00721745812857003));
#14123=CARTESIAN_POINT('',(-0.024585786438,-0.0150942666084793,-0.00541416222200544));
#14124=CARTESIAN_POINT('',(-0.0245857915246626,-0.012237435651537,-0.0103662952709461));
#14125=CARTESIAN_POINT('',(-0.0244999999986063,-0.0115699410488029,-0.0111034454626152));
#14126=CARTESIAN_POINT('',(-0.0244999999986063,-0.0116228081173456,-0.011048357258821));
#14127=CARTESIAN_POINT('',(-0.0245092062722935,-0.0117254136119208,-0.0109395415387983));
#14128=CARTESIAN_POINT('',(-0.0245230015422633,-0.0118068799584357,-0.0108513202198437));
#14129=CARTESIAN_POINT('',(-0.0245385333053876,-0.0118894031339274,-0.0107609585117453));
#14130=CARTESIAN_POINT('',(-0.0245533601934441,-0.0119635583919606,-0.01067822378554));
#14131=CARTESIAN_POINT('',(-0.0245599200212059,-0.0119972700774136,-0.0106403465813125));
#14132=CARTESIAN_POINT('',(-0.0245794719080736,-0.0121054797679643,-0.0105177817029997));
#14133=CARTESIAN_POINT('',(-0.024585786438,-0.0121857364257066,-0.0104241976430973));
#14134=CARTESIAN_POINT('',(-0.024585786438,-0.0122359353199755,-0.0103649372337425));
#14135=CARTESIAN_POINT('',(-0.024499990874883,-0.0115720314953153,-0.011105315051073));
#14136=CARTESIAN_POINT('',(-0.0244999999986063,-0.00383089532186528,-0.0155715855983569));
#14137=CARTESIAN_POINT('',(-0.0244999999986063,-0.0067622055462001,-0.0148504295828433));
#14138=CARTESIAN_POINT('',(-0.0244999999986063,-0.00947974650796292,-0.0132814565763252));
#14139=CARTESIAN_POINT('',(-0.0244999999986063,-0.0115699410488029,-0.0111034454626152));
#14140=CARTESIAN_POINT('',(-0.0244999908693477,-0.00383146949816682,-0.015574332226511));
#14141=CARTESIAN_POINT('',(-0.024585786438,-0.00285833128287572,-0.015779099444879));
#14142=CARTESIAN_POINT('',(-0.024585786438,-0.00293469221286251,-0.0157652669168736));
#14143=CARTESIAN_POINT('',(-0.0245794838828349,-0.00305579558471988,-0.0157425691269049));
#14144=CARTESIAN_POINT('',(-0.0245599357543528,-0.00321605083959362,-0.0157101394805771));
#14145=CARTESIAN_POINT('',(-0.0245533747069374,-0.00326572813265205,-0.0156998793996686));
#14146=CARTESIAN_POINT('',(-0.0245385462192562,-0.00337446747410242,-0.0156770246950493));
#14147=CARTESIAN_POINT('',(-0.0245230204503161,-0.00349393241722351,-0.0156507507466387));
#14148=CARTESIAN_POINT('',(-0.0245092134787734,-0.00361112264764015,-0.0156242982328882));
#14149=CARTESIAN_POINT('',(-0.0244999999986063,-0.00375669803694566,-0.0155898394897091));
#14150=CARTESIAN_POINT('',(-0.0244999999986063,-0.00383089532186528,-0.0155715855983569));
#14151=CARTESIAN_POINT('',(-0.0245857915217653,-0.00285875758549826,-0.0157810767208921));
#14152=CARTESIAN_POINT('',(-0.024585786438,0.,1.40184139924496E-17));
#14153=CARTESIAN_POINT('',(-0.024585786438,-2.56905698753516E-12,-0.0160358983849999));
#14154=CARTESIAN_POINT('',(-0.024585786438,0.00285833128996237,-0.0157790994435952));
#14155=CARTESIAN_POINT('',(-0.024585786438,0.00191577521105279,-0.0159498403367953));
#14156=CARTESIAN_POINT('',(-0.024585786438,0.000957895823969581,-0.0160358983851534));
#14157=CARTESIAN_POINT('',(-0.024585786438,-2.56906054821988E-12,-0.016035898385));
#14158=CARTESIAN_POINT('',(-0.0245857915246446,0.00285875722091595,-0.0157810777871251));
#14159=CARTESIAN_POINT('',(-0.0244999999986063,0.00383089532826959,-0.0155715855967813));
#14160=CARTESIAN_POINT('',(-0.0244999999986063,0.0037567539999507,-0.015589825721817));
#14161=CARTESIAN_POINT('',(-0.0245092062723273,0.00361121406795415,-0.0156242768282245));
#14162=CARTESIAN_POINT('',(-0.024523001542207,0.00349407899314799,-0.0156507180939493));
#14163=CARTESIAN_POINT('',(-0.0245385333055515,0.00337456186892705,-0.0156770044066164));
#14164=CARTESIAN_POINT('',(-0.0245533601931607,0.00326583386869777,-0.0156998573800514));
#14165=CARTESIAN_POINT('',(-0.0245599200213679,0.00321617540143936,-0.0157101139546529));
#14166=CARTESIAN_POINT('',(-0.0245794719079521,0.00305592626012084,-0.01574254385596));
#14167=CARTESIAN_POINT('',(-0.024585786438,0.00293475175703248,-0.0157652561306102));
#14168=CARTESIAN_POINT('',(-0.024585786438,0.00285833128996237,-0.0157790994435952));
#14169=CARTESIAN_POINT('',(-0.0244999908748829,0.00383146920758899,-0.0155743307730475));
#14170=CARTESIAN_POINT('',(-0.0244999999986063,0.0115699410422654,-0.0111034454694274));
#14171=CARTESIAN_POINT('',(-0.0244999999986063,0.00947974650384446,-0.0132814565780498));
#14172=CARTESIAN_POINT('',(-0.0244999999986063,0.00676220554711697,-0.0148504295813392));
#14173=CARTESIAN_POINT('',(-0.0244999999986063,0.00383089532826959,-0.0155715855967813));
#14174=CARTESIAN_POINT('',(-0.0244999908693478,0.01157203260522,-0.0111053160334516));
#14175=CARTESIAN_POINT('',(-0.024585786438,0.0122359353246303,-0.0103649372282474));
#14176=CARTESIAN_POINT('',(-0.024585786438,0.0121857755389782,-0.0104241514694551));
#14177=CARTESIAN_POINT('',(-0.024579483882876,0.01210556701272,-0.0105176811453351));
#14178=CARTESIAN_POINT('',(-0.0245599357542979,0.0119973544631023,-0.010640251472091));
#14179=CARTESIAN_POINT('',(-0.0245533747070335,0.0119636303288962,-0.0106781432259488));
#14180=CARTESIAN_POINT('',(-0.0245385462192108,0.011889467902065,-0.0107608869071751));
#14181=CARTESIAN_POINT('',(-0.0245230204502448,0.0118069815237895,-0.0108512096084395));
#14182=CARTESIAN_POINT('',(-0.0245092134788162,0.0117254778602576,-0.0109394730675282));
#14183=CARTESIAN_POINT('',(-0.0244999999986063,0.0116228480182091,-0.0110483156816441));
#14184=CARTESIAN_POINT('',(-0.0244999999986063,0.0115699410422654,-0.0111034454694274));
#14185=CARTESIAN_POINT('',(-0.0245857915217862,0.0122374350450725,-0.0103662944678227));
#14186=CARTESIAN_POINT('',(-0.024585786438,0.0150942666109112,-0.00541416221522574));
#14187=CARTESIAN_POINT('',(-0.024585786438,0.0144474424349879,-0.00721745812208117));
#14188=CARTESIAN_POINT('',(-0.024585786438,0.0134742233024643,-0.00890312310661903));
#14189=CARTESIAN_POINT('',(-0.024585786438,0.0122359353246303,-0.0103649372282474));
#14190=CARTESIAN_POINT('',(-0.024585791524644,0.0150961928727466,-0.00541478251781387));
#14191=CARTESIAN_POINT('',(-0.0244999999986063,0.0154008363672729,-0.00446814012789783));
#14192=CARTESIAN_POINT('',(-0.0244999999986063,0.0153795621147456,-0.00454146846421457));
#14193=CARTESIAN_POINT('',(-0.0245092062732926,0.0153366276777982,-0.00468473530997678));
#14194=CARTESIAN_POINT('',(-0.0245230015405982,0.0153009589595615,-0.00479939785541512));
#14195=CARTESIAN_POINT('',(-0.0245385332971209,0.0152639650254876,-0.00491604583880081));
#14196=CARTESIAN_POINT('',(-0.0245533602086576,0.0152293922217421,-0.00502163371519752));
#14197=CARTESIAN_POINT('',(-0.0245599200125125,0.0152134455028226,-0.00506976731277923));
#14198=CARTESIAN_POINT('',(-0.0245794719145936,0.0151614060119585,-0.00522476220778196));
#14199=CARTESIAN_POINT('',(-0.024585786438,0.0151204881837907,-0.0053410584927536));
#14200=CARTESIAN_POINT('',(-0.024585786438,0.0150942666109112,-0.00541416221522574));
#14201=CARTESIAN_POINT('',(-0.0244999908750048,0.0154035004811123,-0.0044690164683281));
#14202=CARTESIAN_POINT('',(-0.0244999999986063,0.,1.40374197662062E-17));
#14203=CARTESIAN_POINT('',(-0.0244999908694697,0.0154035018848601,0.00446901694447226));
#14204=CARTESIAN_POINT('',(-0.024585786438,0.0150942666116729,0.00541416221310206));
#14205=CARTESIAN_POINT('',(-0.024585786438,0.015120467756025,0.00534111544375616));
#14206=CARTESIAN_POINT('',(-0.0245794838828001,0.0151613625683128,0.00522488798407675));
#14207=CARTESIAN_POINT('',(-0.0245599357543992,0.0152134053098073,0.00506988800492372));
#14208=CARTESIAN_POINT('',(-0.0245533747068561,0.0152293584647529,0.00502173616910086));
#14209=CARTESIAN_POINT('',(-0.0245385462198197,0.0152639353795454,0.0049161377882726));
#14210=CARTESIAN_POINT('',(-0.0245230204456509,0.0153009139554188,0.004799541102855));
#14211=CARTESIAN_POINT('',(-0.0245092134815725,0.0153366004980514,0.00468482520515153));
#14212=CARTESIAN_POINT('',(-0.0244999999986063,0.0153795460547884,0.00454152381963283));
#14213=CARTESIAN_POINT('',(-0.0244999999986063,0.0154008363636023,0.00446814014054949));
#14214=CARTESIAN_POINT('',(-0.0245857915217865,0.015096191875143,0.00541478239122186));
#14215=CARTESIAN_POINT('',(-0.024585786438,0.0122359353260886,0.0103649372265259));
#14216=CARTESIAN_POINT('',(-0.024585786438,0.0134742233037169,0.0089031231047233));
#14217=CARTESIAN_POINT('',(-0.024585786438,0.0144474424360034,0.0072174581200485));
#14218=CARTESIAN_POINT('',(-0.024585786438,0.0150942666116729,0.00541416221310206));
#14219=CARTESIAN_POINT('',(-0.0245857915246441,0.0122374356535695,0.0103662952685353));
#14220=CARTESIAN_POINT('',(-0.0244999999986063,0.0115699410442475,0.011103445467362));
#14221=CARTESIAN_POINT('',(-0.0244999999986063,0.011622808120127,0.011048357255968));
#14222=CARTESIAN_POINT('',(-0.0245092062752789,0.011725413640156,0.0109395415081673));
#14223=CARTESIAN_POINT('',(-0.0245230015372877,0.0118068799297762,0.0108513202510711));
#14224=CARTESIAN_POINT('',(-0.0245385333071508,0.0118894031377654,0.0107609585074612));
#14225=CARTESIAN_POINT('',(-0.0245533601912659,0.0119635583775685,0.0106782238016603));
#14226=CARTESIAN_POINT('',(-0.0245599200224506,0.0119972700957928,0.0106403465606616));
#14227=CARTESIAN_POINT('',(-0.02457947190714,0.0121054797616445,0.0105177817101086));
#14228=CARTESIAN_POINT('',(-0.024585786438,0.0121857364476053,0.0104241976173165));
#14229=CARTESIAN_POINT('',(-0.024585786438,0.0122359353260886,0.0103649372265259));
#14230=CARTESIAN_POINT('',(-0.0244999908748826,0.0115720314937939,0.0111053150526529));
#14231=CARTESIAN_POINT('',(-0.0244999999986063,0.0038308953154777,0.0155715855999284));
#14232=CARTESIAN_POINT('',(-0.0244999999986063,0.00676220554010803,0.0148504295856173));
#14233=CARTESIAN_POINT('',(-0.0244999999986063,0.00947974650251419,0.0132814565802142));
#14234=CARTESIAN_POINT('',(-0.0244999999986063,0.0115699410442475,0.011103445467362));
#14235=CARTESIAN_POINT('',(-0.0244999908693481,0.00383146949603822,0.0155743322270386));
#14236=CARTESIAN_POINT('',(-0.024585786438,0.00285833127640243,0.0157790994460516));
#14237=CARTESIAN_POINT('',(-0.024585786438,0.00293469221702162,0.0157652669161526));
#14238=CARTESIAN_POINT('',(-0.024579483870863,0.00305579566977372,0.0157425691090143));
#14239=CARTESIAN_POINT('',(-0.0245599357703154,0.00321605070803771,0.0157101395079826));
#14240=CARTESIAN_POINT('',(-0.0245533746790029,0.00326572834549023,0.0156998793552969));
#14241=CARTESIAN_POINT('',(-0.0245385462358954,0.00337446736221416,0.0156770247183708));
#14242=CARTESIAN_POINT('',(-0.024523020440236,0.00349393249877838,0.0156507507289995));
#14243=CARTESIAN_POINT('',(-0.0245092134848215,0.00361112258835951,0.0156242982458343));
#14244=CARTESIAN_POINT('',(-0.0244999999986063,0.00375669803098476,0.0155898394911433));
#14245=CARTESIAN_POINT('',(-0.0244999999986063,0.0038308953154777,0.0155715855999284));
#14246=CARTESIAN_POINT('',(-0.0457000000001119,3.50888490739562E-13,-3.07178390214567E-19));
#14247=CARTESIAN_POINT('',(-0.0460000000003369,3.49584240338238E-13,-2.85957696782259E-19));
#14248=CARTESIAN_POINT('',(-0.0460000000003925,0.0128000000001574,-2.85957696782259E-19));
#14249=CARTESIAN_POINT('',(-0.0245857864382098,-1.06895708554224E-18,5.60523044629629E-12));
#14250=CARTESIAN_POINT('',(-0.026,0.,0.));
#14251=CARTESIAN_POINT('',(-0.0260046754559256,0.00303667233985881,-0.016761340881293));
#14252=CARTESIAN_POINT('',(-0.0260046753764207,-0.00303667205936906,-0.0167613409725091));
#14253=CARTESIAN_POINT('',(-0.0260093507668446,0.00303675796778517,-0.0167595980847489));
#14254=CARTESIAN_POINT('',(-0.0259634000228127,0.00301413112031303,-0.0166352153311787));
#14255=CARTESIAN_POINT('',(-0.0258372476659582,0.00296840214035727,-0.0163834477539786));
#14256=CARTESIAN_POINT('',(-0.0255181562604789,0.00291257308816476,-0.0160777814927587));
#14257=CARTESIAN_POINT('',(-0.0252574621306591,0.00288545817598874,-0.0159300603377363));
#14258=CARTESIAN_POINT('',(-0.0250772590166116,0.00287212279539721,-0.0158591127207493));
#14259=CARTESIAN_POINT('',(-0.0249296521814598,0.0028648507887674,-0.0158197682249595));
#14260=CARTESIAN_POINT('',(-0.0248141730419544,0.0028610453310314,-0.015798524952678));
#14261=CARTESIAN_POINT('',(-0.0247254103202069,0.00285940104998143,-0.0157878998711275));
#14262=CARTESIAN_POINT('',(-0.0246348999596275,0.00285892031357241,-0.0157837419929907));
#14263=CARTESIAN_POINT('',(-0.0246245061620364,0.00285915979859944,-0.0157829616407464));
#14264=CARTESIAN_POINT('',(-0.0245857965998287,0.00285917994845102,-0.0157830567238291));
#14265=CARTESIAN_POINT('',(-0.0245857965941096,-0.00285917916856927,-0.0157830548693243));
#14266=CARTESIAN_POINT('',(-0.024587878063756,-0.00285917808489342,-0.0157830497570209));
#14267=CARTESIAN_POINT('',(-0.0246336063425909,-0.00285921570671322,-0.0157832993187842));
#14268=CARTESIAN_POINT('',(-0.0246879782365064,-0.00285974198593955,-0.0157858384025746));
#14269=CARTESIAN_POINT('',(-0.0247977856685484,-0.00286161612201955,-0.015794835889566));
#14270=CARTESIAN_POINT('',(-0.0249386423726374,-0.0028668146759778,-0.0158199768626178));
#14271=CARTESIAN_POINT('',(-0.0250982101173787,-0.00287617118472857,-0.0158663273977922));
#14272=CARTESIAN_POINT('',(-0.0252906230360713,-0.00289175213210285,-0.0159453481174248));
#14273=CARTESIAN_POINT('',(-0.0254945146967682,-0.00291519894531635,-0.0160683151780273));
#14274=CARTESIAN_POINT('',(-0.0257437244060328,-0.00295515150038263,-0.0162871022461858));
#14275=CARTESIAN_POINT('',(-0.0259279713746338,-0.00300141820559167,-0.0165553620254441));
#14276=CARTESIAN_POINT('',(-0.0259895224206423,-0.00302699365645837,-0.0167059255721978));
#14277=CARTESIAN_POINT('',(-0.0260093506078345,-0.00303675740795554,-0.0167595982669723));
#14278=CARTESIAN_POINT('',(-0.0245415219088105,0.00366437443650513,-0.0171447580070949));
#14279=CARTESIAN_POINT('',(-0.0259961345404699,0.00418903800875609,-0.0170280171879218));
#14280=CARTESIAN_POINT('',(-0.0260208846843343,0.00385989161947845,-0.0167874634655829));
#14281=CARTESIAN_POINT('',(-0.0259763001860542,0.00343771689296902,-0.0166906660659931));
#14282=CARTESIAN_POINT('',(-0.0260105733383942,0.00303746425710906,-0.0167629249983474));
#14283=CARTESIAN_POINT('',(-0.0259980774508458,0.00418905033679694,-0.0170282004945628));
#14284=CARTESIAN_POINT('',(-0.0244999817389186,0.00383204629597067,-0.0155770751715398));
#14285=CARTESIAN_POINT('',(-0.024944756596428,0.00383234583080769,-0.0155784920383265));
#14286=CARTESIAN_POINT('',(-0.0257532661794538,0.00393609475349983,-0.0159769883169212));
#14287=CARTESIAN_POINT('',(-0.0259959930191986,0.00410791207526705,-0.0166992236842379));
#14288=CARTESIAN_POINT('',(-0.0259961548791011,0.00418887289593309,-0.0170282446560903));
#14289=CARTESIAN_POINT('',(-0.0244999999971406,5.18740924496995E-13,-1.35370767904267E-12));
#14290=CARTESIAN_POINT('',(-0.0259999999972629,3.97065401316842E-13,-1.14383970554836E-12));
#14291=CARTESIAN_POINT('',(-0.0259980767575597,0.0126523290853278,-0.0121419242115842));
#14292=CARTESIAN_POINT('',(-0.0259961534925062,0.0126524561027222,-0.012141792577423));
#14293=CARTESIAN_POINT('',(-0.0259959911366752,0.0124079921773759,-0.011907164237172));
#14294=CARTESIAN_POINT('',(-0.0257532552174247,0.0118684248901205,-0.0113972464272905));
#14295=CARTESIAN_POINT('',(-0.0249447500346905,0.0115751992386728,-0.0111081568807122));
#14296=CARTESIAN_POINT('',(-0.024499981727848,0.0115741218908241,-0.0111071889869984));
#14297=CARTESIAN_POINT('',(-0.0245418550974504,0.0130179595803562,-0.0117432056820992));
#14298=CARTESIAN_POINT('',(-0.02601057263116,0.0129983875047157,-0.0110119839056589));
#14299=CARTESIAN_POINT('',(-0.0259762684314703,0.0127354513023962,-0.0113227572395601));
#14300=CARTESIAN_POINT('',(-0.0260208848459058,0.0126084204264453,-0.0117364608404768));
#14301=CARTESIAN_POINT('',(-0.0259961329743928,0.012652176631433,-0.0121418218538705));
#14302=CARTESIAN_POINT('',(-0.0260046753581521,0.0129974109954827,-0.0110105057125223));
#14303=CARTESIAN_POINT('',(-0.0245857965941095,0.0122389368818809,-0.010367649228686));
#14304=CARTESIAN_POINT('',(-0.0245878780633656,0.0122389329963349,-0.010367645734044));
#14305=CARTESIAN_POINT('',(-0.0246336063426967,0.0122391303122479,-0.0103678030963753));
#14306=CARTESIAN_POINT('',(-0.0246879782359766,0.0122410660836794,-0.0103695284094339));
#14307=CARTESIAN_POINT('',(-0.0247977856677001,0.0122479210678728,-0.0103756502023255));
#14308=CARTESIAN_POINT('',(-0.0249386423710321,0.0122670945120445,-0.0103927227684832));
#14309=CARTESIAN_POINT('',(-0.0250982101152105,0.0123025569982902,-0.0104240010100732));
#14310=CARTESIAN_POINT('',(-0.0252906230333307,0.0123632004747365,-0.0104770048657271));
#14311=CARTESIAN_POINT('',(-0.0254945146937632,0.0124579696657952,-0.0105587939314027));
#14312=CARTESIAN_POINT('',(-0.025743724403319,0.0126274685465381,-0.0107027873925713));
#14313=CARTESIAN_POINT('',(-0.0259279713731207,0.0128366549775345,-0.0108769854243933));
#14314=CARTESIAN_POINT('',(-0.0259895224200857,0.0129542591096644,-0.0109744161890341));
#14315=CARTESIAN_POINT('',(-0.0260093506077098,0.0129958591519529,-0.0110097081940201));
#14316=CARTESIAN_POINT('',(-0.0245857864470955,-1.92527892165488E-11,1.05583470944414E-11));
#14317=CARTESIAN_POINT('',(-0.0259999999997638,0.0160355496840746,-0.00575178060268176));
#14318=CARTESIAN_POINT('',(-0.0259999999995772,0.0153483883918416,-0.00766753674812516));
#14319=CARTESIAN_POINT('',(-0.0259999999995979,0.0143144758044963,-0.00945832588025775));
#14320=CARTESIAN_POINT('',(-0.0259999999998258,0.0129989629613864,-0.0110113030887326));
#14321=CARTESIAN_POINT('',(-0.0260046754376191,0.0160340832140701,-0.00575083496141242));
#14322=CARTESIAN_POINT('',(-0.0260093507666748,0.0160326166820256,-0.0057498894970771));
#14323=CARTESIAN_POINT('',(-0.0259634000226623,0.0159135846340675,-0.00570729354502668));
#14324=CARTESIAN_POINT('',(-0.0258372476658943,0.0156726830266146,-0.0056210122147486));
#14325=CARTESIAN_POINT('',(-0.0255181562605256,0.0153800537532759,-0.00551652846150879));
#14326=CARTESIAN_POINT('',(-0.0252574621306131,0.0152385660242035,-0.00546615008668747));
#14327=CARTESIAN_POINT('',(-0.0250772590165566,0.015170455895241,-0.00544222505652501));
#14328=CARTESIAN_POINT('',(-0.0249296521813009,0.0151327465590608,-0.00542885055109215));
#14329=CARTESIAN_POINT('',(-0.0248141730419652,0.0151124466167295,-0.00542152453801596));
#14330=CARTESIAN_POINT('',(-0.0247254103195691,0.0151024228856639,-0.00541763598639992));
#14331=CARTESIAN_POINT('',(-0.0246348999602412,0.0150985816893586,-0.00541597337727203));
#14332=CARTESIAN_POINT('',(-0.0246245061600504,0.0150980256270173,-0.00541537580103899));
#14333=CARTESIAN_POINT('',(-0.0245857965998274,0.0150981180462985,-0.00541540589229385));
#14334=CARTESIAN_POINT('',(-0.0245415219086352,0.016679983194184,-0.00539893765273315));
#14335=CARTESIAN_POINT('',(-0.0259961345406099,0.016841214462651,-0.00488619526152227));
#14336=CARTESIAN_POINT('',(-0.0260209032736197,0.0164680355527262,-0.00505109129460865));
#14337=CARTESIAN_POINT('',(-0.0259762695508448,0.0161735222636546,-0.00536784066556917));
#14338=CARTESIAN_POINT('',(-0.0260105733315168,0.0160358510451588,-0.00575094121468224));
#14339=CARTESIAN_POINT('',(-0.0259980774508441,0.0168413793742882,-0.00488627623713676));
#14340=CARTESIAN_POINT('',(-0.0244999817389172,0.0154061659632965,-0.0044698881448101));
#14341=CARTESIAN_POINT('',(-0.024944756596149,0.015407542773384,-0.00447033717343805));
#14342=CARTESIAN_POINT('',(-0.0257532661791717,0.0158045251349,-0.00457973610997194));
#14343=CARTESIAN_POINT('',(-0.0259959930193616,0.016515907972029,-0.00479205562839269));
#14344=CARTESIAN_POINT('',(-0.0259961548791145,0.0168413289028734,-0.00488645198709862));
#14345=CARTESIAN_POINT('',(-0.0244999999984256,5.24925381567424E-13,-1.62634843653004E-18));
#14346=CARTESIAN_POINT('',(-0.0259999999979621,3.48446901188088E-13,-2.35701788965328E-18));
#14347=CARTESIAN_POINT('',(-0.0259980767574808,0.0168413793587563,0.00488627630154334));
#14348=CARTESIAN_POINT('',(-0.0259961534923684,0.0168413288714539,0.00488645211585265));
#14349=CARTESIAN_POINT('',(-0.025995991136632,0.0165159028049937,0.00479205431631923));
#14350=CARTESIAN_POINT('',(-0.0257532552166203,0.0158045173834629,0.0045797342436974));
#14351=CARTESIAN_POINT('',(-0.0249447500341456,0.0154075456671966,0.00447033815426907));
#14352=CARTESIAN_POINT('',(-0.0244999817278468,0.0154061687726843,0.00446988909050619));
#14353=CARTESIAN_POINT('',(-0.0245418550974137,0.0166788942327279,0.0054022808611622));
#14354=CARTESIAN_POINT('',(-0.026010572631153,0.0160358515601886,0.00575094183466721));
#14355=CARTESIAN_POINT('',(-0.0259762684314615,0.0161735210607565,0.00536784573762992));
#14356=CARTESIAN_POINT('',(-0.0260208848456387,0.0164682834499534,0.00505098197197986));
#14357=CARTESIAN_POINT('',(-0.0259961329744937,0.0168412144868518,0.00488619545012088));
#14358=CARTESIAN_POINT('',(-0.0260046753581802,0.0160340831528961,0.00575083524947786));
#14359=CARTESIAN_POINT('',(-0.02458579659411,0.0150981160505823,0.00541540564052657));
#14360=CARTESIAN_POINT('',(-0.024587878063626,0.0150981110813599,0.00541540402286574));
#14361=CARTESIAN_POINT('',(-0.0246336063429746,0.0150983460190976,0.00541549622229607));
#14362=CARTESIAN_POINT('',(-0.0246879782368823,0.0151008080697915,0.0054163099930172));
#14363=CARTESIAN_POINT('',(-0.0247977856693694,0.0151095371901899,0.00541918568707618));
#14364=CARTESIAN_POINT('',(-0.0249386423737795,0.0151339091886502,0.0054272540938625));
#14365=CARTESIAN_POINT('',(-0.025098210118899,0.015178728184201,0.00544232638726969));
#14366=CARTESIAN_POINT('',(-0.0252906230379044,0.0152549526088682,0.00546834325098496));
#14367=CARTESIAN_POINT('',(-0.0254945146987291,0.0153731686142176,0.00550952124559355));
#14368=CARTESIAN_POINT('',(-0.0257437244077353,0.0155826200512163,0.00558431485227158));
#14369=CARTESIAN_POINT('',(-0.025927971375513,0.0158380731871927,0.00567837659986637));
#14370=CARTESIAN_POINT('',(-0.0259895224208923,0.0159812527677868,0.00573150938270905));
#14371=CARTESIAN_POINT('',(-0.026009350607797,0.0160326165598783,0.00574989007298671));
#14372=CARTESIAN_POINT('',(-0.0245857864470954,-1.92531126805405E-11,-1.05585621839471E-11));
#14373=CARTESIAN_POINT('',(-0.0259999999998258,0.0129989629613864,0.0110113030887327));
#14374=CARTESIAN_POINT('',(-0.0259999999995978,0.0143144758044964,0.00945832588025777));
#14375=CARTESIAN_POINT('',(-0.0259999999995771,0.0153483883918416,0.0076675367481252));
#14376=CARTESIAN_POINT('',(-0.0259999999997637,0.0160355496840746,0.00575178060268182));
#14377=CARTESIAN_POINT('',(-0.0260046754377188,0.0129974107769544,0.0110105059089517));
#14378=CARTESIAN_POINT('',(-0.0260093507668433,0.0129958587141842,0.0110097085877143));
#14379=CARTESIAN_POINT('',(-0.0259634000227723,0.0128994535135814,0.0109279217861875));
#14380=CARTESIAN_POINT('',(-0.0258372476658195,0.0127042808859719,0.0107624355392352));
#14381=CARTESIAN_POINT('',(-0.0255181562605883,0.0124674806650552,0.010561253031256));
#14382=CARTESIAN_POINT('',(-0.0252574621306685,0.0123531078481989,0.0104639102508905));
#14383=CARTESIAN_POINT('',(-0.0250772590166089,0.0122983330998608,0.0104168876640103));
#14384=CARTESIAN_POINT('',(-0.0249296521813909,0.0122678957703277,0.0103909176736192));
#14385=CARTESIAN_POINT('',(-0.0248141730419693,0.0122514012857434,0.0103770004143958));
#14386=CARTESIAN_POINT('',(-0.0247254103198681,0.0122430218357319,0.0103702638844561));
#14387=CARTESIAN_POINT('',(-0.024634899959954,0.0122396613758421,0.01036776861544));
#14388=CARTESIAN_POINT('',(-0.024624506160968,0.0122388658284674,0.0103675858394394));
#14389=CARTESIAN_POINT('',(-0.0245857965998277,0.0122389380979025,0.0103676508312604));
#14390=CARTESIAN_POINT('',(-0.024541521908582,0.0130156087577948,0.0117458203544688));
#14391=CARTESIAN_POINT('',(-0.0259961345402911,0.012652176456026,0.0121418219274446));
#14392=CARTESIAN_POINT('',(-0.026020903273923,0.0126083911539356,0.0117361914938224));
#14393=CARTESIAN_POINT('',(-0.0259762695509608,0.0127354475114188,0.0113227608169304));
#14394=CARTESIAN_POINT('',(-0.0260105733318727,0.012998386710699,0.0110119837691248));
#14395=CARTESIAN_POINT('',(-0.0259980774508218,0.0126523290373502,0.012141924257479));
#14396=CARTESIAN_POINT('',(-0.024499981738918,0.0115741196668296,0.0111071870265766));
#14397=CARTESIAN_POINT('',(-0.0249447565976953,0.0115751969421456,0.0111081548648414));
#14398=CARTESIAN_POINT('',(-0.0257532661814006,0.0118684303832142,0.0113972522082632));
#14399=CARTESIAN_POINT('',(-0.0259959930192577,0.0124079958978922,0.0119071680565776));
#14400=CARTESIAN_POINT('',(-0.0259961548790503,0.0126524560069423,0.0121417926689943));
#14401=CARTESIAN_POINT('',(-0.0244999999971406,5.18764360779374E-13,1.35374416890873E-12));
#14402=CARTESIAN_POINT('',(-0.0259999999972628,3.97088456000253E-13,1.14387320820443E-12));
#14403=CARTESIAN_POINT('',(-0.0259980767575157,0.0041890502732224,0.0170282005132929));
#14404=CARTESIAN_POINT('',(-0.0259961534924216,0.00418887276872869,0.0170282446932658));
#14405=CARTESIAN_POINT('',(-0.0259959911365039,0.00410791062794049,0.0166992185530027));
#14406=CARTESIAN_POINT('',(-0.0257532552162604,0.00393609249381923,0.0159769806701362));
#14407=CARTESIAN_POINT('',(-0.0249447500340041,0.00383234642828381,0.0155784950348394));
#14408=CARTESIAN_POINT('',(-0.0244999817278479,0.00383204688165825,0.015577078077351));
#14409=CARTESIAN_POINT('',(-0.0245418550973269,0.00366093465259704,0.0171454865430141));
#14410=CARTESIAN_POINT('',(-0.0260105726312166,0.00303746405549769,0.0167629257403239));
#14411=CARTESIAN_POINT('',(-0.0259762684315379,0.00343806975865812,0.0166906029764942));
#14412=CARTESIAN_POINT('',(-0.0260208848459788,0.00385986302468689,0.0167874428113377));
#14413=CARTESIAN_POINT('',(-0.0259961329744237,0.00418903785749696,0.0170280173031582));
#14414=CARTESIAN_POINT('',(-0.0260046753582004,0.00303667215730485,0.0167613409619478));
#14415=CARTESIAN_POINT('',(-0.0245857965941096,0.00285917916856925,0.0157830548693242));
#14416=CARTESIAN_POINT('',(-0.025090940149948,0.00285891617560677,0.0157818141848353));
#14417=CARTESIAN_POINT('',(-0.0258263367235061,0.00295388482187573,0.0162565491158958));
#14418=CARTESIAN_POINT('',(-0.0259713996501372,0.00301806968242363,0.0166568692504878));
#14419=CARTESIAN_POINT('',(-0.0260093506078376,0.00303675740795713,0.0167595982669812));
#14420=CARTESIAN_POINT('',(-0.0245857864487112,1.42203703998203E-12,5.38366735710928E-12));
#14421=CARTESIAN_POINT('',(-0.0259999999997604,1.73586899341303E-17,0.0170358983844952));
#14422=CARTESIAN_POINT('',(-0.0259999999997042,0.00101763355997381,0.0170358983845614));
#14423=CARTESIAN_POINT('',(-0.0259999999997053,0.00203524965503534,0.0169444731601271));
#14424=CARTESIAN_POINT('',(-0.0259999999997637,0.00303658672267139,0.0167630836914287));
#14425=CARTESIAN_POINT('',(-0.0260000001248802,-1.15781674900619E-18,0.0170358983847476));
#14426=CARTESIAN_POINT('',(-0.0245857864377007,1.10730438962528E-13,0.0175358983847132));
#14427=CARTESIAN_POINT('',(-0.0245857864487102,-1.42200809927133E-12,5.38360248515839E-12));
#14428=CARTESIAN_POINT('',(-0.0259999999997637,-0.00303658672267143,0.0167630836914286));
#14429=CARTESIAN_POINT('',(-0.0259999999997053,-0.00203524965503538,0.0169444731601271));
#14430=CARTESIAN_POINT('',(-0.0259999999997041,-0.00101763355997385,0.0170358983845614));
#14431=CARTESIAN_POINT('',(-0.0259999999997604,-4.77083853987333E-17,0.0170358983844952));
#14432=CARTESIAN_POINT('',(-0.0260046754377279,-0.00303667243689323,0.0167613408708776));
#14433=CARTESIAN_POINT('',(-0.0260093507668927,-0.00303675796778805,0.0167595980847398));
#14434=CARTESIAN_POINT('',(-0.0259714110358408,-0.00301807586534209,0.0166569001128961));
#14435=CARTESIAN_POINT('',(-0.0258263830287078,-0.00295389696213839,0.0162566051611366));
#14436=CARTESIAN_POINT('',(-0.0250909731285228,-0.00285891698418111,0.0157818158485132));
#14437=CARTESIAN_POINT('',(-0.0245857965998287,-0.0028591799484582,0.0157830567238613));
#14438=CARTESIAN_POINT('',(-0.0245415219087568,-0.00366437443651449,0.0171447580071625));
#14439=CARTESIAN_POINT('',(-0.0259961345404462,-0.00418903800884105,0.0170280171879839));
#14440=CARTESIAN_POINT('',(-0.0260209032740159,-0.00385964439988298,0.0167872827872964));
#14441=CARTESIAN_POINT('',(-0.0259762695510075,-0.00343807475236031,0.0166906014821321));
#14442=CARTESIAN_POINT('',(-0.0260105733318218,-0.0030374643344677,0.0167629249843816));
#14443=CARTESIAN_POINT('',(-0.0259980774508371,-0.00418905033688052,0.0170282004946286));
#14444=CARTESIAN_POINT('',(-0.0244999817389183,-0.00383204629596097,0.0155770751714919));
#14445=CARTESIAN_POINT('',(-0.0249447565965779,-0.0038323458308052,0.0155784920383121));
#14446=CARTESIAN_POINT('',(-0.0257532661796553,-0.00393609475357222,0.015976988317185));
#14447=CARTESIAN_POINT('',(-0.0259959930191771,-0.0041079120753024,0.0166992236843931));
#14448=CARTESIAN_POINT('',(-0.0259961548790839,-0.0041888728959336,0.0170282446561009));
#14449=CARTESIAN_POINT('',(-0.0244999999971407,-5.18631834631121E-13,1.35352719870077E-12));
#14450=CARTESIAN_POINT('',(-0.025999999997263,-3.96961679161639E-13,1.14366711529932E-12));
#14451=CARTESIAN_POINT('',(-0.0259980767575473,-0.0126523290853398,0.0121419242116851));
#14452=CARTESIAN_POINT('',(-0.0259961534924817,-0.0126524561027242,0.012141792577421));
#14453=CARTESIAN_POINT('',(-0.0259959911366461,-0.012407992177481,0.0119071642372684));
#14454=CARTESIAN_POINT('',(-0.0257532552176058,-0.0118684248903005,0.011397246427474));
#14455=CARTESIAN_POINT('',(-0.0249447500348285,-0.0115751992386655,0.0111081568807063));
#14456=CARTESIAN_POINT('',(-0.0244999817278477,-0.011574121890793,0.011107188986971));
#14457=CARTESIAN_POINT('',(-0.0245418550974116,-0.0130179595803988,0.0117432056821331));
#14458=CARTESIAN_POINT('',(-0.0260105726312484,-0.0129983875048527,0.0110119839054969));
#14459=CARTESIAN_POINT('',(-0.0259762684314917,-0.0127354513024245,0.0113227572394375));
#14460=CARTESIAN_POINT('',(-0.0260208848459214,-0.0126084204264179,0.0117364608404772));
#14461=CARTESIAN_POINT('',(-0.0259961329743619,-0.0126521766314437,0.0121418218539703));
#14462=CARTESIAN_POINT('',(-0.0260046753581827,-0.0129974109956148,0.0110105057123484));
#14463=CARTESIAN_POINT('',(-0.0245857965941096,-0.0122389368819011,0.0103676492287045));
#14464=CARTESIAN_POINT('',(-0.0250909401471701,-0.0122379939140726,0.0103668011278518));
#14465=CARTESIAN_POINT('',(-0.0258263367195619,-0.0126016420976086,0.0106864138505677));
#14466=CARTESIAN_POINT('',(-0.0259713996491344,-0.01291623707483,0.010942159639068));
#14467=CARTESIAN_POINT('',(-0.0260093506077712,-0.0129958591519313,0.0110097081940098));
#14468=CARTESIAN_POINT('',(-0.0245857864470955,1.92530944572749E-11,-1.05585582240299E-11));
#14469=CARTESIAN_POINT('',(-0.0259999999997637,-0.0160355496840745,0.00575178060268177));
#14470=CARTESIAN_POINT('',(-0.0259999999995771,-0.0153483883918416,0.00766753674812515));
#14471=CARTESIAN_POINT('',(-0.0259999999995978,-0.0143144758044963,0.00945832588025774));
#14472=CARTESIAN_POINT('',(-0.0259999999998258,-0.0129989629613864,0.0110113030887326));
#14473=CARTESIAN_POINT('',(-0.0260046754376107,-0.0160340832137518,0.0057508349623088));
#14474=CARTESIAN_POINT('',(-0.0260093507666581,-0.0160326166820308,0.00574988949708065));
#14475=CARTESIAN_POINT('',(-0.025971411035752,-0.0159343365787225,0.0057147196865982));
#14476=CARTESIAN_POINT('',(-0.0258263830290665,-0.0155555815303819,0.00557015277131583));
#14477=CARTESIAN_POINT('',(-0.025090973128876,-0.015096911934659,0.00541501318838743));
#14478=CARTESIAN_POINT('',(-0.0245857965998274,-0.0150981180463038,0.00541540589229551));
#14479=CARTESIAN_POINT('',(-0.0245415219086213,-0.0166799831941954,0.00539893765274277));
#14480=CARTESIAN_POINT('',(-0.0259961345406086,-0.0168412144627859,0.00488619526146272));
#14481=CARTESIAN_POINT('',(-0.0260209032736532,-0.0164680355525104,0.00505109129466021));
#14482=CARTESIAN_POINT('',(-0.0259762695507925,-0.016173522263216,0.00536784066603291));
#14483=CARTESIAN_POINT('',(-0.0260105733315772,-0.0160358510448399,0.0057509412155698));
#14484=CARTESIAN_POINT('',(-0.0259980774508479,-0.0168413793744232,0.00488627623707682));
#14485=CARTESIAN_POINT('',(-0.0244999817389172,-0.0154061659632896,0.00446988814480776));
#14486=CARTESIAN_POINT('',(-0.024944756596158,-0.0154075427733792,0.00447033717343636));
#14487=CARTESIAN_POINT('',(-0.0257532661791859,-0.0158045251349107,0.0045797361099757));
#14488=CARTESIAN_POINT('',(-0.025995993019367,-0.0165159079720358,0.00479205562839404));
#14489=CARTESIAN_POINT('',(-0.0259961548791221,-0.0168413289028737,0.00488645198709787));
#14490=CARTESIAN_POINT('',(-0.0244999999984257,-5.24694626034855E-13,7.65719141414477E-19));
#14491=CARTESIAN_POINT('',(-0.0259999999979621,-3.48223200806651E-13,4.6127030534049E-19));
#14492=CARTESIAN_POINT('',(-0.0259980767574809,-0.0168413793586215,-0.00488627630160291));
#14493=CARTESIAN_POINT('',(-0.0259961534923684,-0.0168413288714539,-0.00488645211585266));
#14494=CARTESIAN_POINT('',(-0.025995991136632,-0.0165159028049937,-0.00479205431631923));
#14495=CARTESIAN_POINT('',(-0.0257532552166203,-0.0158045173834629,-0.00457973424369741));
#14496=CARTESIAN_POINT('',(-0.0249447500341456,-0.0154075456671966,-0.00447033815426907));
#14497=CARTESIAN_POINT('',(-0.0244999817278467,-0.0154061687726844,-0.00446988909050619));
#14498=CARTESIAN_POINT('',(-0.0245418550974135,-0.0166788942327286,-0.00540228086116028));
#14499=CARTESIAN_POINT('',(-0.0260105726311714,-0.0160358515601145,-0.00575094183487335));
#14500=CARTESIAN_POINT('',(-0.0259762684314567,-0.0161735210606341,-0.00536784573779487));
#14501=CARTESIAN_POINT('',(-0.0260208848456298,-0.0164682834498121,-0.00505098197208591));
#14502=CARTESIAN_POINT('',(-0.0259961329745026,-0.0168412144867175,-0.00488619545018022));
#14503=CARTESIAN_POINT('',(-0.0260046753581802,-0.0160340831528214,-0.00575083524968604));
#14504=CARTESIAN_POINT('',(-0.02458579659411,-0.0150981160505823,-0.00541540564052657));
#14505=CARTESIAN_POINT('',(-0.0250909401516257,-0.0150969100897713,-0.00541501305685423));
#14506=CARTESIAN_POINT('',(-0.0258263367258225,-0.015555526925824,-0.0055701352631442));
#14507=CARTESIAN_POINT('',(-0.0259713996506763,-0.0159343067607731,-0.00571470961034891));
#14508=CARTESIAN_POINT('',(-0.026009350607797,-0.0160326165598783,-0.00574989007298672));
#14509=CARTESIAN_POINT('',(-0.0245857864470955,1.92527724721921E-11,1.05583478911826E-11));
#14510=CARTESIAN_POINT('',(-0.0259999999998258,-0.0129989629613864,-0.0110113030887327));
#14511=CARTESIAN_POINT('',(-0.0259999999995979,-0.0143144758044963,-0.00945832588025778));
#14512=CARTESIAN_POINT('',(-0.0259999999995772,-0.0153483883918416,-0.00766753674812521));
#14513=CARTESIAN_POINT('',(-0.0259999999997638,-0.0160355496840745,-0.00575178060268184));
#14514=CARTESIAN_POINT('',(-0.0260046754377188,-0.0129974107760712,-0.0110105059099944));
#14515=CARTESIAN_POINT('',(-0.0260093507668434,-0.0129958587141842,-0.0110097085877143));
#14516=CARTESIAN_POINT('',(-0.0259714110351495,-0.0129162607116119,-0.0109421804253578));
#14517=CARTESIAN_POINT('',(-0.0258263830259916,-0.0126016845651491,-0.0106864523879323));
#14518=CARTESIAN_POINT('',(-0.0250909731266351,-0.0122379949504956,-0.0103668026598678));
#14519=CARTESIAN_POINT('',(-0.0245857965998277,-0.0122389380979025,-0.0103676508312604));
#14520=CARTESIAN_POINT('',(-0.0245415219085822,-0.0130156087577962,-0.0117458203544672));
#14521=CARTESIAN_POINT('',(-0.0259961345402822,-0.0126521764560418,-0.0121418219275906));
#14522=CARTESIAN_POINT('',(-0.0260209032739087,-0.0126083911539552,-0.0117361914943769));
#14523=CARTESIAN_POINT('',(-0.0259762695510121,-0.0127354475110793,-0.0113227608179002));
#14524=CARTESIAN_POINT('',(-0.0260105733317587,-0.0129983867098248,-0.011011983770158));
#14525=CARTESIAN_POINT('',(-0.0259980774508218,-0.012652329037366,-0.0121419242576256));
#14526=CARTESIAN_POINT('',(-0.024499981738918,-0.0115741196668296,-0.0111071870265765));
#14527=CARTESIAN_POINT('',(-0.0249447565976953,-0.0115751969421456,-0.0111081548648414));
#14528=CARTESIAN_POINT('',(-0.0257532661814006,-0.0118684303832142,-0.0113972522082632));
#14529=CARTESIAN_POINT('',(-0.0259959930192577,-0.0124079958978922,-0.0119071680565776));
#14530=CARTESIAN_POINT('',(-0.0259961548790503,-0.0126524560069422,-0.0121417926689943));
#14531=CARTESIAN_POINT('',(-0.0244999999971407,-5.18644711631284E-13,-1.35354294616328E-12));
#14532=CARTESIAN_POINT('',(-0.025999999997263,-3.9697401421664E-13,-1.14368187585572E-12));
#14533=CARTESIAN_POINT('',(-0.0259980767575158,-0.00418905027313784,-0.0170282005132274));
#14534=CARTESIAN_POINT('',(-0.0259961534924215,-0.00418887276872622,-0.0170282446932557));
#14535=CARTESIAN_POINT('',(-0.0259959911365014,-0.00410791062793844,-0.0166992185529941));
#14536=CARTESIAN_POINT('',(-0.0257532552162551,-0.00393609249381833,-0.0159769806701326));
#14537=CARTESIAN_POINT('',(-0.0249447500340021,-0.00383234642828381,-0.0155784950348394));
#14538=CARTESIAN_POINT('',(-0.0244999817278479,-0.00383204688165824,-0.015577078077351));
#14539=CARTESIAN_POINT('',(-0.0245418550973269,-0.00366093465259706,-0.0171454865430142));
#14540=CARTESIAN_POINT('',(-0.0260105726395446,-0.00303746395823507,-0.0167629257578844));
#14541=CARTESIAN_POINT('',(-0.0259762952739958,-0.00343775617407728,-0.0166906595617935));
#14542=CARTESIAN_POINT('',(-0.026020876834144,-0.00385996963576985,-0.0167875207162035));
#14543=CARTESIAN_POINT('',(-0.0259961329724585,-0.00418903788362998,-0.0170280173222573));
#14544=CARTESIAN_POINT('',(-0.046,4.85722573273506E-19,3.46944695195362E-20));
#14545=CARTESIAN_POINT('',(-0.0460000000004017,-1.91988200481306E-13,-2.26738972774339E-20));
#14546=CARTESIAN_POINT('',(-0.0460000000004512,0.0157358983848686,-2.26738972774339E-20));
#14547=CARTESIAN_POINT('',(-0.019,0.,0.));
#14548=CARTESIAN_POINT('',(-0.02600000025,0.00303658672694563,-0.016763083691069));
#14549=CARTESIAN_POINT('',(-0.027000000125,0.00303658672694563,-0.016763083691069));
#14550=CARTESIAN_POINT('',(-0.028,0.00303658672694563,-0.016763083691069));
#14551=CARTESIAN_POINT('',(-0.028999999875,0.00303658672694563,-0.016763083691069));
#14552=CARTESIAN_POINT('',(-0.028999999875,0.00303658672474891,-0.0167630836915008));
#14553=CARTESIAN_POINT('',(-0.029,-0.00303658672393521,-0.0167630836916143));
#14554=CARTESIAN_POINT('',(-0.0280000000833333,-0.00303658672393521,-0.0167630836916143));
#14555=CARTESIAN_POINT('',(-0.0270000001666667,-0.00303658672393521,-0.0167630836916143));
#14556=CARTESIAN_POINT('',(-0.02600000025,-0.00303658672393521,-0.0167630836916143));
#14557=CARTESIAN_POINT('',(-0.029,-0.00303658672114831,-0.016763083692153));
#14558=CARTESIAN_POINT('',(-0.029,0.,0.));
#14559=CARTESIAN_POINT('',(-0.019,0.003303956249,-0.018239062532));
#14560=CARTESIAN_POINT('',(-0.029,0.003303956249,-0.018239062532));
#14561=CARTESIAN_POINT('',(-0.0289999998749999,0.00436461653820612,-0.0171784024646543));
#14562=CARTESIAN_POINT('',(-0.02899999975,0.00436461642035826,-0.0171784023597986));
#14563=CARTESIAN_POINT('',(-0.0279999999166667,0.00436461642035826,-0.0171784023597986));
#14564=CARTESIAN_POINT('',(-0.0270000000833333,0.00436461642035826,-0.0171784023597986));
#14565=CARTESIAN_POINT('',(-0.02600000025,0.00436461642035826,-0.0171784023597986));
#14566=CARTESIAN_POINT('',(-0.026,0.00436461886889965,-0.0171784047953479));
#14567=CARTESIAN_POINT('',(-0.026,0.003303956249,-0.018239062532));
#14568=CARTESIAN_POINT('',(-0.026,-2.55351295663786E-17,-2.63677968348474E-18));
#14569=CARTESIAN_POINT('',(-0.0260000000001354,-1.37314950086772E-13,2.61821090022989E-18));
#14570=CARTESIAN_POINT('',(-0.0260000000000933,0.0329999999999944,2.61821090022989E-18));
#14571=CARTESIAN_POINT('',(-0.026,0.00436461672182346,0.0171784026352795));
#14572=CARTESIAN_POINT('',(-0.026,0.00545695029196146,0.0182707362276815));
#14573=CARTESIAN_POINT('',(-0.026,0.00654928386209946,0.0193630698200835));
#14574=CARTESIAN_POINT('',(-0.026,0.00764161743223745,0.0204554034124854));
#14575=CARTESIAN_POINT('',(-0.026000000125,0.00436461642085125,0.0171784023602916));
#14576=CARTESIAN_POINT('',(-0.0260000001249999,0.00764161753161064,0.0204554034909548));
#14577=CARTESIAN_POINT('',(-0.026,0.003303956249,0.018239062532));
#14578=CARTESIAN_POINT('',(-0.026,0.014143513369,0.011980841311));
#14579=CARTESIAN_POINT('',(-0.0260000001249999,0.0126946255340264,0.0123690732293488));
#14580=CARTESIAN_POINT('',(-0.026,0.0138940902881418,0.0168455365833053));
#14581=CARTESIAN_POINT('',(-0.026,0.0134942687055029,0.0153533821314328));
#14582=CARTESIAN_POINT('',(-0.026,0.0130944471228641,0.0138612276795603));
#14583=CARTESIAN_POINT('',(-0.026,0.0126946255402253,0.0123690732276878));
#14584=CARTESIAN_POINT('',(-0.026000000125,0.013894090320796,0.0168455367788748));
#14585=CARTESIAN_POINT('',(-0.026,0.01534297906,0.016457308211));
#14586=CARTESIAN_POINT('',(-0.026000000125,0.016365844330921,0.0175544620917123));
#14587=CARTESIAN_POINT('',(-0.026,0.,0.));
#14588=CARTESIAN_POINT('',(-0.026000000125,0.0233855322877997,0.00539600589483076));
#14589=CARTESIAN_POINT('',(-0.026,0.021923936519,0.00505875553));
#14590=CARTESIAN_POINT('',(-0.0260000001249999,0.0215357078290251,0.00360986683636835));
#14591=CARTESIAN_POINT('',(-0.026,0.0170592414781658,0.00480933239988356));
#14592=CARTESIAN_POINT('',(-0.026,0.0185513968874907,0.00440951056069614));
#14593=CARTESIAN_POINT('',(-0.026,0.0200435522968155,0.00400968872150873));
#14594=CARTESIAN_POINT('',(-0.026,0.0215357077061403,0.00360986688232132));
#14595=CARTESIAN_POINT('',(-0.026000000125,0.0170592410507286,0.00480933248146393));
#14596=CARTESIAN_POINT('',(-0.026,0.017447469618,0.006258221221));
#14597=CARTESIAN_POINT('',(-0.026,0.017447469618,-0.006258221221));
#14598=CARTESIAN_POINT('',(-0.0260000001249999,0.0170592444030468,-0.00480933159968851));
#14599=CARTESIAN_POINT('',(-0.026,0.0215357077103104,-0.00360986688120394));
#14600=CARTESIAN_POINT('',(-0.026,0.0200435532759288,-0.00400968845915609));
#14601=CARTESIAN_POINT('',(-0.026,0.0185513988415473,-0.00440951003710825));
#14602=CARTESIAN_POINT('',(-0.026,0.0170592444071657,-0.0048093316150604));
#14603=CARTESIAN_POINT('',(-0.026000000125,0.0215357079510786,-0.00360986679080852));
#14604=CARTESIAN_POINT('',(-0.026,0.021923936519,-0.00505875553));
#14605=CARTESIAN_POINT('',(-0.026000000125,0.0233855322869016,-0.00539600589872286));
#14606=CARTESIAN_POINT('',(-0.026,0.,0.));
#14607=CARTESIAN_POINT('',(-0.026000000125,0.0163658443295185,-0.0175544620930199));
#14608=CARTESIAN_POINT('',(-0.026,0.01534297906,-0.016457308211));
#14609=CARTESIAN_POINT('',(-0.0260000001249999,0.013894090297154,-0.0168455366541086));
#14610=CARTESIAN_POINT('',(-0.026,0.0126946247563403,-0.0123690703021891));
#14611=CARTESIAN_POINT('',(-0.026,0.0130944465955277,-0.013861225711514));
#14612=CARTESIAN_POINT('',(-0.026,0.0134942684347151,-0.015353381120839));
#14613=CARTESIAN_POINT('',(-0.026,0.0138940902739026,-0.0168455365301639));
#14614=CARTESIAN_POINT('',(-0.026000000125,0.012694624629357,-0.0123690698778722));
#14615=CARTESIAN_POINT('',(-0.026,0.014143513369,-0.011980841311));
#14616=CARTESIAN_POINT('',(-0.026,0.00764161743223745,-0.0204554034124855));
#14617=CARTESIAN_POINT('',(-0.026,0.00654928457995689,-0.0193630705379409));
#14618=CARTESIAN_POINT('',(-0.026,0.00545695172767632,-0.0182707376633963));
#14619=CARTESIAN_POINT('',(-0.026,0.00436461887539576,-0.0171784047888518));
#14620=CARTESIAN_POINT('',(-0.026000000125,0.00764161763081172,-0.0204554035695319));
#14621=CARTESIAN_POINT('',(-0.026,0.006580957459,-0.021516063741));
#14622=CARTESIAN_POINT('',(-0.026000000125,0.00701968795640335,-0.0229504679905696));
#14623=CARTESIAN_POINT('',(-0.026,0.,0.));
#14624=CARTESIAN_POINT('',(-0.026000000125,-0.00701968795550563,-0.0229504679908442));
#14625=CARTESIAN_POINT('',(-0.026,-0.006580957459,-0.021516063741));
#14626=CARTESIAN_POINT('',(-0.0260000001249999,-0.0076416175313931,-0.0204554034907373));
#14627=CARTESIAN_POINT('',(-0.026,-0.00436461672182347,-0.0171784026352795));
#14628=CARTESIAN_POINT('',(-0.026,-0.00545695029196146,-0.0182707362276815));
#14629=CARTESIAN_POINT('',(-0.026,-0.00654928386209946,-0.0193630698200835));
#14630=CARTESIAN_POINT('',(-0.026,-0.00764161743223745,-0.0204554034124855));
#14631=CARTESIAN_POINT('',(-0.026000000125,-0.00436461642041616,-0.0171784023598565));
#14632=CARTESIAN_POINT('',(-0.026,-0.003303956249,-0.018239062532));
#14633=CARTESIAN_POINT('',(-0.026,-0.014143513369,-0.011980841311));
#14634=CARTESIAN_POINT('',(-0.0260000001249999,-0.0126946255341409,-0.0123690732297761));
#14635=CARTESIAN_POINT('',(-0.026,-0.0138940902739026,-0.0168455365301639));
#14636=CARTESIAN_POINT('',(-0.026,-0.0134942686960483,-0.0153533820961476));
#14637=CARTESIAN_POINT('',(-0.026,-0.013094447118194,-0.0138612276621313));
#14638=CARTESIAN_POINT('',(-0.026,-0.0126946255403397,-0.0123690732281151));
#14639=CARTESIAN_POINT('',(-0.026000000125,-0.01389409032085,-0.0168455367790761));
#14640=CARTESIAN_POINT('',(-0.026,-0.01534297906,-0.016457308211));
#14641=CARTESIAN_POINT('',(-0.026000000125,-0.0163658443305974,-0.017554462092014));
#14642=CARTESIAN_POINT('',(-0.026,0.,0.));
#14643=CARTESIAN_POINT('',(-0.026000000125,-0.0233855322862084,-0.00539600590172708));
#14644=CARTESIAN_POINT('',(-0.026,-0.021923936519,-0.00505875553));
#14645=CARTESIAN_POINT('',(-0.0260000001249999,-0.0215357078306828,-0.00360986683592415));
#14646=CARTESIAN_POINT('',(-0.026,-0.0170592414781658,-0.00480933239988355));
#14647=CARTESIAN_POINT('',(-0.026,-0.0185513968888807,-0.00440951056032368));
#14648=CARTESIAN_POINT('',(-0.026,-0.0200435522995956,-0.00400968872076381));
#14649=CARTESIAN_POINT('',(-0.026,-0.0215357077103104,-0.00360986688120394));
#14650=CARTESIAN_POINT('',(-0.026000000125,-0.0170592410498741,-0.0048093324816929));
#14651=CARTESIAN_POINT('',(-0.026,-0.017447469618,-0.006258221221));
#14652=CARTESIAN_POINT('',(-0.026,-0.017447469618,0.006258221221));
#14653=CARTESIAN_POINT('',(-0.0260000001249999,-0.0170592444034741,0.00480933159957403));
#14654=CARTESIAN_POINT('',(-0.026,-0.0215357077061403,0.00360986688232132));
#14655=CARTESIAN_POINT('',(-0.026,-0.0200435532732912,0.00400968845986285));
#14656=CARTESIAN_POINT('',(-0.026,-0.0185513988404421,0.00440951003740437));
#14657=CARTESIAN_POINT('',(-0.026,-0.017059244407593,0.0048093316149459));
#14658=CARTESIAN_POINT('',(-0.026000000125,-0.0215357079515059,0.00360986679069403));
#14659=CARTESIAN_POINT('',(-0.026,-0.021923936519,0.00505875553));
#14660=CARTESIAN_POINT('',(-0.026000000125,-0.0233855322868325,0.00539600589902264));
#14661=CARTESIAN_POINT('',(-0.026,0.,0.));
#14662=CARTESIAN_POINT('',(-0.026000000125,-0.0163658443346953,0.0175544620881936));
#14663=CARTESIAN_POINT('',(-0.026,-0.01534297906,0.016457308211));
#14664=CARTESIAN_POINT('',(-0.0260000001249999,-0.0138940903043532,0.0168455366809765));
#14665=CARTESIAN_POINT('',(-0.026,-0.0126946247563402,0.0123690703021891));
#14666=CARTESIAN_POINT('',(-0.026,-0.0130944466002741,0.0138612257292278));
#14667=CARTESIAN_POINT('',(-0.026,-0.0134942684442079,0.0153533811562665));
#14668=CARTESIAN_POINT('',(-0.026,-0.0138940902881418,0.0168455365833052));
#14669=CARTESIAN_POINT('',(-0.026000000125,-0.0126946246295162,0.0123690698784665));
#14670=CARTESIAN_POINT('',(-0.026,-0.014143513369,0.011980841311));
#14671=CARTESIAN_POINT('',(-0.026,-0.003303956249,0.018239062532));
#14672=CARTESIAN_POINT('',(-0.0260000001249999,-0.00436461886924978,0.017178404795698));
#14673=CARTESIAN_POINT('',(-0.026,-0.00764161743223745,0.0204554034124854));
#14674=CARTESIAN_POINT('',(-0.026,-0.00654928458007359,0.0193630705380576));
#14675=CARTESIAN_POINT('',(-0.026,-0.00545695172790972,0.0182707376636298));
#14676=CARTESIAN_POINT('',(-0.026,-0.00436461887574586,0.0171784047892019));
#14677=CARTESIAN_POINT('',(-0.026000000125,-0.00764161763077926,0.0204554035694995));
#14678=CARTESIAN_POINT('',(-0.026,-0.006580957459,0.021516063741));
#14679=CARTESIAN_POINT('',(-0.026000000125,-0.00701968795610915,0.0229504679906597));
#14680=CARTESIAN_POINT('',(-0.026,0.,0.));
#14681=CARTESIAN_POINT('',(-0.026000000125,0.00701968795079842,0.022950467992284));
#14682=CARTESIAN_POINT('',(-0.026,0.006580957459,0.021516063741));
#14683=CARTESIAN_POINT('',(-0.026,0.027720932313,-0.010089594228));
#14684=CARTESIAN_POINT('',(-0.026,0.027720932313,-0.011389594228));
#14685=CARTESIAN_POINT('',(-0.026,0.022598311072,-0.018962234486));
#14686=CARTESIAN_POINT('',(-0.026,0.022598311072,-0.020262234486));
#14687=CARTESIAN_POINT('',(-0.026,0.01475,-0.025547749412));
#14688=CARTESIAN_POINT('',(-0.026,0.01475,-0.026847749412));
#14689=CARTESIAN_POINT('',(-0.026,0.005122621241,-0.029051828714));
#14690=CARTESIAN_POINT('',(-0.026,0.005122621241,-0.030351828714));
#14691=CARTESIAN_POINT('',(-0.026,-0.005122621241,-0.029051828714));
#14692=CARTESIAN_POINT('',(-0.026,-0.005122621241,-0.030351828714));
#14693=CARTESIAN_POINT('',(-0.026,-0.01475,-0.025547749412));
#14694=CARTESIAN_POINT('',(-0.026,-0.01475,-0.026847749412));
#14695=CARTESIAN_POINT('',(-0.026,-0.022598311072,-0.018962234486));
#14696=CARTESIAN_POINT('',(-0.026,-0.022598311072,-0.020262234486));
#14697=CARTESIAN_POINT('',(-0.026,-0.027720932313,-0.010089594228));
#14698=CARTESIAN_POINT('',(-0.026,-0.027720932313,-0.011389594228));
#14699=CARTESIAN_POINT('',(-0.026,-0.0295,0.));
#14700=CARTESIAN_POINT('',(-0.026,-0.0295,-0.0013));
#14701=CARTESIAN_POINT('',(-0.026,-0.027720932313,0.010089594228));
#14702=CARTESIAN_POINT('',(-0.026,-0.027720932313,0.008789594228));
#14703=CARTESIAN_POINT('',(-0.026,-0.022598311072,0.018962234486));
#14704=CARTESIAN_POINT('',(-0.026,-0.022598311072,0.017662234486));
#14705=CARTESIAN_POINT('',(-0.026,-0.01475,0.025547749412));
#14706=CARTESIAN_POINT('',(-0.026,-0.01475,0.024247749412));
#14707=CARTESIAN_POINT('',(-0.026,-0.005122621241,0.029051828714));
#14708=CARTESIAN_POINT('',(-0.026,-0.005122621241,0.027751828714));
#14709=CARTESIAN_POINT('',(-0.026,0.005122621241,0.029051828714));
#14710=CARTESIAN_POINT('',(-0.026,0.005122621241,0.027751828714));
#14711=CARTESIAN_POINT('',(-0.026,0.01475,0.025547749412));
#14712=CARTESIAN_POINT('',(-0.026,0.01475,0.024247749412));
#14713=CARTESIAN_POINT('',(-0.026,0.022598311072,0.018962234486));
#14714=CARTESIAN_POINT('',(-0.026,0.022598311072,0.017662234486));
#14715=CARTESIAN_POINT('',(-0.026,0.027720932313,0.010089594228));
#14716=CARTESIAN_POINT('',(-0.026,0.027720932313,0.008789594228));
#14717=CARTESIAN_POINT('',(-0.026,0.0295,0.));
#14718=CARTESIAN_POINT('',(-0.026,0.0295,-0.0013));
#14719=CARTESIAN_POINT('',(-0.019,0.014143513369,-0.011980841311));
#14720=CARTESIAN_POINT('',(-0.02600000025,0.0126946246294055,-0.0123690698780533));
#14721=CARTESIAN_POINT('',(-0.0270000000833333,0.0126946246294055,-0.0123690698780533));
#14722=CARTESIAN_POINT('',(-0.0279999999166667,0.0126946246294055,-0.0123690698780533));
#14723=CARTESIAN_POINT('',(-0.02899999975,0.0126946246294055,-0.0123690698780533));
#14724=CARTESIAN_POINT('',(-0.029,0.0126946246726379,-0.0123690700146031));
#14725=CARTESIAN_POINT('',(-0.029,0.014143513369,-0.011980841311));
#14726=CARTESIAN_POINT('',(-0.028999999875,0.012998962961142,-0.0110113030890252));
#14727=CARTESIAN_POINT('',(-0.028999999875,0.0129989629609766,-0.0110113030892194));
#14728=CARTESIAN_POINT('',(-0.028,0.0129989629609766,-0.0110113030892194));
#14729=CARTESIAN_POINT('',(-0.027000000125,0.0129989629609766,-0.0110113030892194));
#14730=CARTESIAN_POINT('',(-0.02600000025,0.0129989629609766,-0.0110113030892194));
#14731=CARTESIAN_POINT('',(-0.019,0.,0.));
#14732=CARTESIAN_POINT('',(-0.02600000025,0.0160355496845724,-0.00575178060235749));
#14733=CARTESIAN_POINT('',(-0.027000000125,0.0160355496845724,-0.00575178060235749));
#14734=CARTESIAN_POINT('',(-0.028,0.0160355496845724,-0.00575178060235749));
#14735=CARTESIAN_POINT('',(-0.028999999875,0.0160355496845724,-0.00575178060235749));
#14736=CARTESIAN_POINT('',(-0.028999999875,0.016035549684198,-0.00575178060272061));
#14737=CARTESIAN_POINT('',(-0.029,0.,0.));
#14738=CARTESIAN_POINT('',(-0.019,0.017447469618,-0.006258221221));
#14739=CARTESIAN_POINT('',(-0.029,0.017447469618,-0.006258221221));
#14740=CARTESIAN_POINT('',(-0.0289999998749999,0.0170592411886433,-0.00480933246098534));
#14741=CARTESIAN_POINT('',(-0.02899999975,0.017059241049795,-0.0048093324817141));
#14742=CARTESIAN_POINT('',(-0.0279999999166667,0.017059241049795,-0.0048093324817141));
#14743=CARTESIAN_POINT('',(-0.0270000000833333,0.017059241049795,-0.0048093324817141));
#14744=CARTESIAN_POINT('',(-0.02600000025,0.017059241049795,-0.0048093324817141));
#14745=CARTESIAN_POINT('',(-0.019,0.017447469618,0.006258221221));
#14746=CARTESIAN_POINT('',(-0.02600000025,0.0170592410509098,0.0048093324814154));
#14747=CARTESIAN_POINT('',(-0.0270000000833333,0.0170592410509098,0.0048093324814154));
#14748=CARTESIAN_POINT('',(-0.0279999999166667,0.0170592410509098,0.0048093324814154));
#14749=CARTESIAN_POINT('',(-0.02899999975,0.0170592410509098,0.0048093324814154));
#14750=CARTESIAN_POINT('',(-0.029,0.0170592411890195,0.00480933246088452));
#14751=CARTESIAN_POINT('',(-0.029,0.017447469618,0.006258221221));
#14752=CARTESIAN_POINT('',(-0.028999999875,0.0160355496840715,0.00575178060307333));
#14753=CARTESIAN_POINT('',(-0.028999999875,0.0160355496838868,0.00575178060290777));
#14754=CARTESIAN_POINT('',(-0.028,0.0160355496838868,0.00575178060290777));
#14755=CARTESIAN_POINT('',(-0.027000000125,0.0160355496838868,0.00575178060290777));
#14756=CARTESIAN_POINT('',(-0.02600000025,0.0160355496838868,0.00575178060290777));
#14757=CARTESIAN_POINT('',(-0.019,0.,0.));
#14758=CARTESIAN_POINT('',(-0.029,0.,0.));
#14759=CARTESIAN_POINT('',(-0.028999999875,0.0129989629621973,0.0110113030877919));
#14760=CARTESIAN_POINT('',(-0.02600000025,0.0129989629630871,0.0110113030867529));
#14761=CARTESIAN_POINT('',(-0.027000000125,0.0129989629630871,0.0110113030867529));
#14762=CARTESIAN_POINT('',(-0.028,0.0129989629630871,0.0110113030867529));
#14763=CARTESIAN_POINT('',(-0.028999999875,0.0129989629630871,0.0110113030867529));
#14764=CARTESIAN_POINT('',(-0.019,0.014143513369,0.011980841311));
#14765=CARTESIAN_POINT('',(-0.029,0.014143513369,0.011980841311));
#14766=CARTESIAN_POINT('',(-0.0289999998749999,0.0126946246727312,0.0123690700149513));
#14767=CARTESIAN_POINT('',(-0.02899999975,0.012694624629495,0.0123690698783874));
#14768=CARTESIAN_POINT('',(-0.0279999999166667,0.012694624629495,0.0123690698783874));
#14769=CARTESIAN_POINT('',(-0.0270000000833333,0.012694624629495,0.0123690698783874));
#14770=CARTESIAN_POINT('',(-0.02600000025,0.012694624629495,0.0123690698783874));
#14771=CARTESIAN_POINT('',(-0.019,0.003303956249,0.018239062532));
#14772=CARTESIAN_POINT('',(-0.02600000025,0.00436461642098383,0.0171784023604242));
#14773=CARTESIAN_POINT('',(-0.0270000000833333,0.00436461642098383,0.0171784023604242));
#14774=CARTESIAN_POINT('',(-0.0279999999166667,0.00436461642098383,0.0171784023604242));
#14775=CARTESIAN_POINT('',(-0.02899999975,0.00436461642098383,0.0171784023604242));
#14776=CARTESIAN_POINT('',(-0.029,0.00436461651612127,0.0171784024425695));
#14777=CARTESIAN_POINT('',(-0.029,0.003303956249,0.018239062532));
#14778=CARTESIAN_POINT('',(-0.028999999875,0.00303658672248485,0.0167630836919108));
#14779=CARTESIAN_POINT('',(-0.028999999875,0.00303658672242937,0.0167630836919547));
#14780=CARTESIAN_POINT('',(-0.028,0.00303658672242937,0.0167630836919547));
#14781=CARTESIAN_POINT('',(-0.027000000125,0.00303658672242937,0.0167630836919547));
#14782=CARTESIAN_POINT('',(-0.02600000025,0.00303658672242937,0.0167630836919547));
#14783=CARTESIAN_POINT('',(-0.019,0.,0.));
#14784=CARTESIAN_POINT('',(-0.029,0.,0.));
#14785=CARTESIAN_POINT('',(-0.028999999875,-0.00303658672131075,0.0167630836921236));
#14786=CARTESIAN_POINT('',(-0.02600000025,-0.0030365867200693,0.0167630836923146));
#14787=CARTESIAN_POINT('',(-0.027000000125,-0.0030365867200693,0.0167630836923146));
#14788=CARTESIAN_POINT('',(-0.028,-0.0030365867200693,0.0167630836923146));
#14789=CARTESIAN_POINT('',(-0.028999999875,-0.0030365867200693,0.0167630836923146));
#14790=CARTESIAN_POINT('',(-0.019,-0.003303956249,0.018239062532));
#14791=CARTESIAN_POINT('',(-0.029,-0.003303956249,0.018239062532));
#14792=CARTESIAN_POINT('',(-0.0289999998749999,-0.00436461651615862,0.0171784024426068));
#14793=CARTESIAN_POINT('',(-0.02899999975,-0.00436461642079335,0.0171784023602337));
#14794=CARTESIAN_POINT('',(-0.0279999999166667,-0.00436461642079335,0.0171784023602337));
#14795=CARTESIAN_POINT('',(-0.0270000000833333,-0.00436461642079335,0.0171784023602337));
#14796=CARTESIAN_POINT('',(-0.02600000025,-0.00436461642079335,0.0171784023602337));
#14797=CARTESIAN_POINT('',(-0.019,-0.014143513369,0.011980841311));
#14798=CARTESIAN_POINT('',(-0.02600000025,-0.0126946246295647,0.0123690698786476));
#14799=CARTESIAN_POINT('',(-0.0270000000833333,-0.0126946246295647,0.0123690698786476));
#14800=CARTESIAN_POINT('',(-0.0279999999166667,-0.0126946246295647,0.0123690698786476));
#14801=CARTESIAN_POINT('',(-0.02899999975,-0.0126946246295647,0.0123690698786476));
#14802=CARTESIAN_POINT('',(-0.029,-0.0126946246727175,0.0123690700149003));
#14803=CARTESIAN_POINT('',(-0.029,-0.014143513369,0.011980841311));
#14804=CARTESIAN_POINT('',(-0.028999999875,-0.0129989629614279,0.0110113030886876));
#14805=CARTESIAN_POINT('',(-0.028999999875,-0.0129989629615484,0.0110113030885444));
#14806=CARTESIAN_POINT('',(-0.028,-0.0129989629615484,0.0110113030885444));
#14807=CARTESIAN_POINT('',(-0.027000000125,-0.0129989629615484,0.0110113030885444));
#14808=CARTESIAN_POINT('',(-0.02600000025,-0.0129989629615484,0.0110113030885444));
#14809=CARTESIAN_POINT('',(-0.019,0.,0.));
#14810=CARTESIAN_POINT('',(-0.029,0.,0.));
#14811=CARTESIAN_POINT('',(-0.028999999875,-0.0160355496830183,0.00575178060600955));
#14812=CARTESIAN_POINT('',(-0.02600000025,-0.016035549682213,0.00575178060893538));
#14813=CARTESIAN_POINT('',(-0.027000000125,-0.016035549682213,0.00575178060893538));
#14814=CARTESIAN_POINT('',(-0.028,-0.016035549682213,0.00575178060893538));
#14815=CARTESIAN_POINT('',(-0.028999999875,-0.016035549682213,0.00575178060893538));
#14816=CARTESIAN_POINT('',(-0.019,-0.017447469618,0.006258221221));
#14817=CARTESIAN_POINT('',(-0.029,-0.017447469618,0.006258221221));
#14818=CARTESIAN_POINT('',(-0.0289999998749999,-0.0170592411890706,0.00480933246087085));
#14819=CARTESIAN_POINT('',(-0.02899999975,-0.0170592410506495,0.00480933248148512));
#14820=CARTESIAN_POINT('',(-0.0279999999166667,-0.0170592410506495,0.00480933248148512));
#14821=CARTESIAN_POINT('',(-0.0270000000833333,-0.0170592410506495,0.00480933248148512));
#14822=CARTESIAN_POINT('',(-0.02600000025,-0.0170592410506495,0.00480933248148512));
#14823=CARTESIAN_POINT('',(-0.019,-0.017447469618,-0.006258221221));
#14824=CARTESIAN_POINT('',(-0.02600000025,-0.0170592410500552,-0.00480933248164437));
#14825=CARTESIAN_POINT('',(-0.0270000000833333,-0.0170592410500552,-0.00480933248164437));
#14826=CARTESIAN_POINT('',(-0.0279999999166667,-0.0170592410500552,-0.00480933248164437));
#14827=CARTESIAN_POINT('',(-0.02899999975,-0.0170592410500552,-0.00480933248164437));
#14828=CARTESIAN_POINT('',(-0.029,-0.0170592411885923,-0.00480933246099901));
#14829=CARTESIAN_POINT('',(-0.029,-0.017447469618,-0.006258221221));
#14830=CARTESIAN_POINT('',(-0.028999999875,-0.0160355496839222,-0.0057517806034897));
#14831=CARTESIAN_POINT('',(-0.028999999875,-0.0160355496835881,-0.00575178060374051));
#14832=CARTESIAN_POINT('',(-0.028,-0.0160355496835881,-0.00575178060374051));
#14833=CARTESIAN_POINT('',(-0.027000000125,-0.0160355496835881,-0.00575178060374051));
#14834=CARTESIAN_POINT('',(-0.02600000025,-0.0160355496835881,-0.00575178060374051));
#14835=CARTESIAN_POINT('',(-0.019,0.,0.));
#14836=CARTESIAN_POINT('',(-0.02600000025,-0.0129989629565927,-0.0110113030944196));
#14837=CARTESIAN_POINT('',(-0.027000000125,-0.0129989629565927,-0.0110113030944196));
#14838=CARTESIAN_POINT('',(-0.028,-0.0129989629565927,-0.0110113030944196));
#14839=CARTESIAN_POINT('',(-0.028999999875,-0.0129989629565927,-0.0110113030944196));
#14840=CARTESIAN_POINT('',(-0.028999999875,-0.0129989629589501,-0.0110113030916253));
#14841=CARTESIAN_POINT('',(-0.029,0.,0.));
#14842=CARTESIAN_POINT('',(-0.019,-0.014143513369,-0.011980841311));
#14843=CARTESIAN_POINT('',(-0.029,-0.014143513369,-0.011980841311));
#14844=CARTESIAN_POINT('',(-0.0289999998749999,-0.0126946246728457,-0.0123690700153786));
#14845=CARTESIAN_POINT('',(-0.02899999975,-0.012694624629724,-0.012369069879242));
#14846=CARTESIAN_POINT('',(-0.0279999999166667,-0.012694624629724,-0.012369069879242));
#14847=CARTESIAN_POINT('',(-0.0270000000833333,-0.012694624629724,-0.012369069879242));
#14848=CARTESIAN_POINT('',(-0.02600000025,-0.012694624629724,-0.012369069879242));
#14849=CARTESIAN_POINT('',(-0.019,-0.003303956249,-0.018239062532));
#14850=CARTESIAN_POINT('',(-0.029,-0.003303956249,-0.018239062532));
#14851=CARTESIAN_POINT('',(-0.0289999998749999,-0.00436461653816879,-0.017178402464617));
#14852=CARTESIAN_POINT('',(-0.02600000025,-0.00436461642054874,-0.0171784023599891));
#14853=CARTESIAN_POINT('',(-0.0270000000833333,-0.00436461642054874,-0.0171784023599891));
#14854=CARTESIAN_POINT('',(-0.0279999999166667,-0.00436461642054874,-0.0171784023599891));
#14855=CARTESIAN_POINT('',(-0.02899999975,-0.00436461642054874,-0.0171784023599891));
#14856=CARTESIAN_POINT('',(-0.0457000000004547,-1.9104357969811E-13,2.14962800695782E-20));
#14857=CARTESIAN_POINT('',(-0.0457000000001921,1.91044680793333E-13,3.0529103015044E-19));
#14858=CARTESIAN_POINT('',(-0.0456999998751711,-1.43991496994606E-12,0.0160358983847874));
#14859=CARTESIAN_POINT('',(-0.0456999998750961,-1.19492304347938E-11,-0.0160358983847874));
#14860=CARTESIAN_POINT('',(-0.0457000000001922,-1.19492250689532E-11,-0.0160358983845747));
#14861=CARTESIAN_POINT('',(-0.0457000000001856,-0.00209909420135277,-0.0160358983830355));
#14862=CARTESIAN_POINT('',(-0.0457000000001723,-0.00629630402788561,-0.0152009391640093));
#14863=CARTESIAN_POINT('',(-0.0457000000001555,-0.0116343304668846,-0.0116342951457853));
#14864=CARTESIAN_POINT('',(-0.0457000000001443,-0.0152009290827189,-0.00629643515766662));
#14865=CARTESIAN_POINT('',(-0.0457000000001404,-0.0164533830368208,5.39146857913628E-12));
#14866=CARTESIAN_POINT('',(-0.0457000000001443,-0.0152009290785924,0.00629643516762871));
#14867=CARTESIAN_POINT('',(-0.0457000000001555,-0.0116343304592599,0.01163429515341));
#14868=CARTESIAN_POINT('',(-0.0457000000001724,-0.00629630401792351,0.0152009391681357));
#14869=CARTESIAN_POINT('',(-0.0457000000001856,-0.00209909419084346,0.0160358983844112));
#14870=CARTESIAN_POINT('',(-0.0457000000001922,-1.4399100356034E-12,0.0160358983845747));
#14871=CARTESIAN_POINT('',(-0.029,-2.55351295663786E-17,2.63677968348474E-18));
#14872=CARTESIAN_POINT('',(-0.0289999999998646,-1.37316647958235E-13,2.1453454169561E-18));
#14873=CARTESIAN_POINT('',(-0.0289999999999067,0.0329999999999944,2.1453454169561E-18));
#14874=CARTESIAN_POINT('',(-0.0289999999996631,3.49860794609214E-13,-3.47956526835693E-19));
#14875=CARTESIAN_POINT('',(-0.0289999999996075,0.0163358983851577,-3.47956526835693E-19));
#14876=CARTESIAN_POINT('',(-0.029,0.021923936519,-0.00505875553));
#14877=CARTESIAN_POINT('',(-0.029,0.021535705976621,-0.00360986733288895));
#14878=CARTESIAN_POINT('',(-0.028999999875,0.0233855322869173,-0.00539600589872648));
#14879=CARTESIAN_POINT('',(-0.029,0.0170592413274916,-0.00480933244025659));
#14880=CARTESIAN_POINT('',(-0.029,0.0185513962116061,-0.00440951074179888));
#14881=CARTESIAN_POINT('',(-0.029,0.0200435510957205,-0.00400968904334117));
#14882=CARTESIAN_POINT('',(-0.029,0.0215357059798349,-0.00360986734488346));
#14883=CARTESIAN_POINT('',(-0.029,0.0138940902739026,-0.0168455365301639));
#14884=CARTESIAN_POINT('',(-0.029,0.0134942684212575,-0.0153533810706144));
#14885=CARTESIAN_POINT('',(-0.029,0.0130944465686124,-0.0138612256110648));
#14886=CARTESIAN_POINT('',(-0.029,0.0126946247159673,-0.0123690701515153));
#14887=CARTESIAN_POINT('',(-0.02899999975,0.013894090320454,-0.0168455367782344));
#14888=CARTESIAN_POINT('',(-0.029,0.01534297906,-0.016457308211));
#14889=CARTESIAN_POINT('',(-0.028999999875,0.0163658443296136,-0.0175544620931219));
#14890=CARTESIAN_POINT('',(-0.029,0.,0.));
#14891=CARTESIAN_POINT('',(-0.029,0.0215357077061403,0.00360986688232131));
#14892=CARTESIAN_POINT('',(-0.029,0.0200435522465908,0.0040096887349664));
#14893=CARTESIAN_POINT('',(-0.029,0.0185513967870412,0.00440951058761149));
#14894=CARTESIAN_POINT('',(-0.029,0.0170592413274916,0.00480933244025658));
#14895=CARTESIAN_POINT('',(-0.02899999975,0.0215357079520908,0.00360986679036687));
#14896=CARTESIAN_POINT('',(-0.029,0.021923936519,0.00505875553));
#14897=CARTESIAN_POINT('',(-0.028999999875,0.0233855322877841,0.00539600589482715));
#14898=CARTESIAN_POINT('',(-0.029,0.,0.));
#14899=CARTESIAN_POINT('',(-0.028999999875,0.0163658443308259,0.0175544620916103));
#14900=CARTESIAN_POINT('',(-0.029,0.01534297906,0.016457308211));
#14901=CARTESIAN_POINT('',(-0.029,0.0138940903045709,0.0168455366811526));
#14902=CARTESIAN_POINT('',(-0.029,0.0126946247159673,0.0123690701515152));
#14903=CARTESIAN_POINT('',(-0.029,0.0130944465733588,0.0138612256287786));
#14904=CARTESIAN_POINT('',(-0.029,0.0134942684307503,0.0153533811060419));
#14905=CARTESIAN_POINT('',(-0.029,0.0138940902881418,0.0168455365833053));
#14906=CARTESIAN_POINT('',(-0.029,0.00764161743223745,0.0204554034124855));
#14907=CARTESIAN_POINT('',(-0.029,0.00654928382533293,0.0193630697833169));
#14908=CARTESIAN_POINT('',(-0.029,0.0054569502184284,0.0182707361541484));
#14909=CARTESIAN_POINT('',(-0.029,0.00436461661152387,0.0171784025249799));
#14910=CARTESIAN_POINT('',(-0.02899999975,0.00764161763111642,0.0204554035695568));
#14911=CARTESIAN_POINT('',(-0.029,0.006580957459,0.021516063741));
#14912=CARTESIAN_POINT('',(-0.028999999875,0.0070196879508506,0.0229504679924546));
#14913=CARTESIAN_POINT('',(-0.029,0.,0.));
#14914=CARTESIAN_POINT('',(-0.028999999875,-0.00701968795605696,0.022950467990489));
#14915=CARTESIAN_POINT('',(-0.029,-0.006580957459,0.021516063741));
#14916=CARTESIAN_POINT('',(-0.029,-0.00764161753161873,0.0204554034912427));
#14917=CARTESIAN_POINT('',(-0.029,-0.00436461661152388,0.0171784025249799));
#14918=CARTESIAN_POINT('',(-0.029,-0.00545695021842841,0.0182707361541484));
#14919=CARTESIAN_POINT('',(-0.029,-0.00654928382533293,0.0193630697833169));
#14920=CARTESIAN_POINT('',(-0.029,-0.00764161743223745,0.0204554034124855));
#14921=CARTESIAN_POINT('',(-0.029,-0.0138940902881418,0.0168455365833053));
#14922=CARTESIAN_POINT('',(-0.029,-0.0134942684307503,0.0153533811060419));
#14923=CARTESIAN_POINT('',(-0.029,-0.0130944465733588,0.0138612256287786));
#14924=CARTESIAN_POINT('',(-0.029,-0.0126946247159673,0.0123690701515152));
#14925=CARTESIAN_POINT('',(-0.02899999975,-0.0138940903206133,0.0168455367788287));
#14926=CARTESIAN_POINT('',(-0.029,-0.01534297906,0.016457308211));
#14927=CARTESIAN_POINT('',(-0.028999999875,-0.0163658443347904,0.0175544620882956));
#14928=CARTESIAN_POINT('',(-0.029,0.,0.));
#14929=CARTESIAN_POINT('',(-0.028999999875,-0.0233855322868481,0.00539600589902625));
#14930=CARTESIAN_POINT('',(-0.029,-0.021923936519,0.00505875553));
#14931=CARTESIAN_POINT('',(-0.029,-0.0215357078285702,0.00360986683666066));
#14932=CARTESIAN_POINT('',(-0.029,-0.0170592413274916,0.00480933244025658));
#14933=CARTESIAN_POINT('',(-0.029,-0.0185513967870412,0.00440951058761149));
#14934=CARTESIAN_POINT('',(-0.029,-0.0200435522465908,0.0040096887349664));
#14935=CARTESIAN_POINT('',(-0.029,-0.0215357077061403,0.00360986688232131));
#14936=CARTESIAN_POINT('',(-0.029,-0.0215357077103104,-0.00360986688120393));
#14937=CARTESIAN_POINT('',(-0.029,-0.0200435522493708,-0.00400968873422149));
#14938=CARTESIAN_POINT('',(-0.029,-0.0185513967884312,-0.00440951058723904));
#14939=CARTESIAN_POINT('',(-0.029,-0.0170592413274916,-0.0048093324402566));
#14940=CARTESIAN_POINT('',(-0.02899999975,-0.0215357079512363,-0.00360986679059585));
#14941=CARTESIAN_POINT('',(-0.029,-0.021923936519,-0.00505875553));
#14942=CARTESIAN_POINT('',(-0.028999999875,-0.0233855322861928,-0.00539600590172346));
#14943=CARTESIAN_POINT('',(-0.029,0.,0.));
#14944=CARTESIAN_POINT('',(-0.028999999875,-0.0163658443305024,-0.017554462091912));
#14945=CARTESIAN_POINT('',(-0.029,-0.01534297906,-0.016457308211));
#14946=CARTESIAN_POINT('',(-0.029,-0.0138940902974513,-0.0168455366545819));
#14947=CARTESIAN_POINT('',(-0.029,-0.0126946247159673,-0.0123690701515153));
#14948=CARTESIAN_POINT('',(-0.029,-0.0130944465686124,-0.0138612256110648));
#14949=CARTESIAN_POINT('',(-0.029,-0.0134942684212575,-0.0153533810706144));
#14950=CARTESIAN_POINT('',(-0.029,-0.0138940902739026,-0.0168455365301639));
#14951=CARTESIAN_POINT('',(-0.029,0.006580957459,-0.021516063741));
#14952=CARTESIAN_POINT('',(-0.029,0.00764161753161873,-0.0204554034912427));
#14953=CARTESIAN_POINT('',(-0.028999999875,0.00701968795635117,-0.022950467990399));
#14954=CARTESIAN_POINT('',(-0.029,0.00436461665605399,-0.01717840256951));
#14955=CARTESIAN_POINT('',(-0.029,0.00545695024811515,-0.0182707361838351));
#14956=CARTESIAN_POINT('',(-0.029,0.0065492838401763,-0.0193630697981603));
#14957=CARTESIAN_POINT('',(-0.029,0.00764161743223745,-0.0204554034124854));
#14958=CARTESIAN_POINT('',(-0.029,-0.00764161743223745,-0.0204554034124854));
#14959=CARTESIAN_POINT('',(-0.029,-0.0065492838401763,-0.0193630697981603));
#14960=CARTESIAN_POINT('',(-0.029,-0.00545695024811515,-0.0182707361838351));
#14961=CARTESIAN_POINT('',(-0.029,-0.004364616656054,-0.01717840256951));
#14962=CARTESIAN_POINT('',(-0.02899999975,-0.00764161763068133,-0.0204554035691217));
#14963=CARTESIAN_POINT('',(-0.029,-0.006580957459,-0.021516063741));
#14964=CARTESIAN_POINT('',(-0.028999999875,-0.00701968795555781,-0.0229504679910148));
#14965=CARTESIAN_POINT('',(-0.029,0.,0.));
#14966=CARTESIAN_POINT('',(-0.029,0.027720932313,-0.010089594228));
#14967=CARTESIAN_POINT('',(-0.029,0.027720932313,-0.011389594228));
#14968=CARTESIAN_POINT('',(-0.029,0.022598311072,-0.018962234486));
#14969=CARTESIAN_POINT('',(-0.029,0.022598311072,-0.020262234486));
#14970=CARTESIAN_POINT('',(-0.029,0.01475,-0.025547749412));
#14971=CARTESIAN_POINT('',(-0.029,0.01475,-0.026847749412));
#14972=CARTESIAN_POINT('',(-0.029,0.005122621241,-0.029051828714));
#14973=CARTESIAN_POINT('',(-0.029,0.005122621241,-0.030351828714));
#14974=CARTESIAN_POINT('',(-0.029,-0.005122621241,-0.029051828714));
#14975=CARTESIAN_POINT('',(-0.029,-0.005122621241,-0.030351828714));
#14976=CARTESIAN_POINT('',(-0.029,-0.01475,-0.025547749412));
#14977=CARTESIAN_POINT('',(-0.029,-0.01475,-0.026847749412));
#14978=CARTESIAN_POINT('',(-0.029,-0.022598311072,-0.018962234486));
#14979=CARTESIAN_POINT('',(-0.029,-0.022598311072,-0.020262234486));
#14980=CARTESIAN_POINT('',(-0.029,-0.027720932313,-0.010089594228));
#14981=CARTESIAN_POINT('',(-0.029,-0.027720932313,-0.011389594228));
#14982=CARTESIAN_POINT('',(-0.029,-0.0295,0.));
#14983=CARTESIAN_POINT('',(-0.029,-0.0295,-0.0013));
#14984=CARTESIAN_POINT('',(-0.029,-0.027720932313,0.010089594228));
#14985=CARTESIAN_POINT('',(-0.029,-0.027720932313,0.008789594228));
#14986=CARTESIAN_POINT('',(-0.029,-0.022598311072,0.018962234486));
#14987=CARTESIAN_POINT('',(-0.029,-0.022598311072,0.017662234486));
#14988=CARTESIAN_POINT('',(-0.029,-0.01475,0.025547749412));
#14989=CARTESIAN_POINT('',(-0.029,-0.01475,0.024247749412));
#14990=CARTESIAN_POINT('',(-0.029,-0.005122621241,0.029051828714));
#14991=CARTESIAN_POINT('',(-0.029,-0.005122621241,0.027751828714));
#14992=CARTESIAN_POINT('',(-0.029,0.005122621241,0.029051828714));
#14993=CARTESIAN_POINT('',(-0.029,0.005122621241,0.027751828714));
#14994=CARTESIAN_POINT('',(-0.029,0.01475,0.025547749412));
#14995=CARTESIAN_POINT('',(-0.029,0.01475,0.024247749412));
#14996=CARTESIAN_POINT('',(-0.029,0.022598311072,0.018962234486));
#14997=CARTESIAN_POINT('',(-0.029,0.022598311072,0.017662234486));
#14998=CARTESIAN_POINT('',(-0.029,0.027720932313,0.010089594228));
#14999=CARTESIAN_POINT('',(-0.029,0.027720932313,0.008789594228));
#15000=CARTESIAN_POINT('',(-0.029,0.0295,0.));
#15001=CARTESIAN_POINT('',(-0.029,0.0295,-0.0013));
#15002=CARTESIAN_POINT('',(-0.0275,0.006003117026,-0.018816902965));
#15003=CARTESIAN_POINT('',(-0.026000000125,0.007641617631,-0.02045540357));
#15004=CARTESIAN_POINT('',(-0.0270000000833333,0.007641617631,-0.02045540357));
#15005=CARTESIAN_POINT('',(-0.0280000000416667,0.007641617631,-0.02045540357));
#15006=CARTESIAN_POINT('',(-0.029,0.007641617631,-0.02045540357));
#15007=CARTESIAN_POINT('',(-0.046,0.0295,0.));
#15008=CARTESIAN_POINT('',(-0.046,0.027720932313,0.010089594228));
#15009=CARTESIAN_POINT('',(-0.046,0.022598311072,0.018962234486));
#15010=CARTESIAN_POINT('',(-0.046,0.01475,0.025547749412));
#15011=CARTESIAN_POINT('',(-0.046,0.005122621241,0.029051828714));
#15012=CARTESIAN_POINT('',(-0.046,-0.005122621241,0.029051828714));
#15013=CARTESIAN_POINT('',(-0.046,-0.01475,0.025547749412));
#15014=CARTESIAN_POINT('',(-0.046,-0.022598311072,0.018962234486));
#15015=CARTESIAN_POINT('',(-0.046,-0.027720932313,0.010089594228));
#15016=CARTESIAN_POINT('',(-0.046,-0.0295,0.));
#15017=CARTESIAN_POINT('',(-0.046,-0.027720932313,-0.010089594228));
#15018=CARTESIAN_POINT('',(-0.046,-0.022598311072,-0.018962234486));
#15019=CARTESIAN_POINT('',(-0.046,-0.01475,-0.025547749412));
#15020=CARTESIAN_POINT('',(-0.046,-0.005122621241,-0.029051828714));
#15021=CARTESIAN_POINT('',(-0.046,0.005122621241,-0.029051828714));
#15022=CARTESIAN_POINT('',(-0.046,0.01475,-0.025547749412));
#15023=CARTESIAN_POINT('',(-0.046,0.022598311072,-0.018962234486));
#15024=CARTESIAN_POINT('',(-0.046,0.027720932313,-0.010089594228));
#15025=CARTESIAN_POINT('',(-0.0275,0.0132943574755,0.0146073033285));
#15026=CARTESIAN_POINT('',(-0.026000000125,0.013894090321,0.016845536779));
#15027=CARTESIAN_POINT('',(-0.0270000000833333,0.013894090321,0.016845536779));
#15028=CARTESIAN_POINT('',(-0.0280000000416667,0.013894090321,0.016845536779));
#15029=CARTESIAN_POINT('',(-0.029,0.013894090321,0.016845536779));
#15030=CARTESIAN_POINT('',(-0.019,0.01534297906,0.016457308211));
#15031=CARTESIAN_POINT('',(-0.02899999975,0.0163658443309724,0.0175544620914737));
#15032=CARTESIAN_POINT('',(-0.0279999999166667,0.0163658443309724,0.0175544620914737));
#15033=CARTESIAN_POINT('',(-0.0270000000833333,0.0163658443309724,0.0175544620914737));
#15034=CARTESIAN_POINT('',(-0.02600000025,0.0163658443309724,0.0175544620914737));
#15035=CARTESIAN_POINT('',(-0.019,0.,0.));
#15036=CARTESIAN_POINT('',(-0.02899999975,0.0233855322886682,0.00539600589099533));
#15037=CARTESIAN_POINT('',(-0.0279999999166667,0.0233855322886682,0.00539600589099533));
#15038=CARTESIAN_POINT('',(-0.0270000000833333,0.0233855322886682,0.00539600589099533));
#15039=CARTESIAN_POINT('',(-0.02600000025,0.0233855322886682,0.00539600589099533));
#15040=CARTESIAN_POINT('',(-0.019,0.021923936519,0.00505875553));
#15041=CARTESIAN_POINT('',(-0.02899999975,0.0215357079519098,0.0036098667904154));
#15042=CARTESIAN_POINT('',(-0.0279999999166667,0.0215357079519098,0.0036098667904154));
#15043=CARTESIAN_POINT('',(-0.0270000000833333,0.0215357079519098,0.0036098667904154));
#15044=CARTESIAN_POINT('',(-0.02600000025,0.0215357079519098,0.0036098667904154));
#15045=CARTESIAN_POINT('',(-0.0275,0.019297474501,0.00420959963649999));
#15046=CARTESIAN_POINT('',(-0.0275,0.019297474501,-0.00420959963649999));
#15047=CARTESIAN_POINT('',(-0.026000000125,0.021535707951,-0.00360986679099999));
#15048=CARTESIAN_POINT('',(-0.0270000000833333,0.021535707951,-0.00360986679099999));
#15049=CARTESIAN_POINT('',(-0.0280000000416667,0.021535707951,-0.00360986679099999));
#15050=CARTESIAN_POINT('',(-0.029,0.021535707951,-0.00360986679099999));
#15051=CARTESIAN_POINT('',(-0.019,0.021923936519,-0.00505875553));
#15052=CARTESIAN_POINT('',(-0.02899999975,0.0233855322869034,-0.00539600589878677));
#15053=CARTESIAN_POINT('',(-0.0279999999166667,0.0233855322869034,-0.00539600589878677));
#15054=CARTESIAN_POINT('',(-0.0270000000833333,0.0233855322869034,-0.00539600589878677));
#15055=CARTESIAN_POINT('',(-0.02600000025,0.0233855322869034,-0.00539600589878677));
#15056=CARTESIAN_POINT('',(-0.019,0.,0.));
#15057=CARTESIAN_POINT('',(-0.02899999975,0.0163658443283577,-0.0175544620942928));
#15058=CARTESIAN_POINT('',(-0.0279999999166667,0.0163658443283577,-0.0175544620942928));
#15059=CARTESIAN_POINT('',(-0.0270000000833333,0.0163658443283577,-0.0175544620942928));
#15060=CARTESIAN_POINT('',(-0.02600000025,0.0163658443283577,-0.0175544620942928));
#15061=CARTESIAN_POINT('',(-0.019,0.01534297906,-0.016457308211));
#15062=CARTESIAN_POINT('',(-0.02899999975,0.0138940903204055,-0.0168455367780533));
#15063=CARTESIAN_POINT('',(-0.0279999999166667,0.0138940903204055,-0.0168455367780533));
#15064=CARTESIAN_POINT('',(-0.0270000000833333,0.0138940903204055,-0.0168455367780533));
#15065=CARTESIAN_POINT('',(-0.02600000025,0.0138940903204055,-0.0168455367780533));
#15066=CARTESIAN_POINT('',(-0.0275,0.0132943574755,-0.0146073033285));
#15067=CARTESIAN_POINT('',(-0.019,0.006580957459,-0.021516063741));
#15068=CARTESIAN_POINT('',(-0.02899999975,0.0070196879564287,-0.0229504679903753));
#15069=CARTESIAN_POINT('',(-0.0279999999166667,0.0070196879564287,-0.0229504679903753));
#15070=CARTESIAN_POINT('',(-0.0270000000833333,0.0070196879564287,-0.0229504679903753));
#15071=CARTESIAN_POINT('',(-0.02600000025,0.0070196879564287,-0.0229504679903753));
#15072=CARTESIAN_POINT('',(-0.019,0.,0.));
#15073=CARTESIAN_POINT('',(-0.02899999975,-0.00701968795473764,-0.0229504679912657));
#15074=CARTESIAN_POINT('',(-0.0279999999166667,-0.00701968795473764,-0.0229504679912657));
#15075=CARTESIAN_POINT('',(-0.0270000000833333,-0.00701968795473764,-0.0229504679912657));
#15076=CARTESIAN_POINT('',(-0.02600000025,-0.00701968795473764,-0.0229504679912657));
#15077=CARTESIAN_POINT('',(-0.019,-0.006580957459,-0.021516063741));
#15078=CARTESIAN_POINT('',(-0.02899999975,-0.00764161763054874,-0.0204554035689891));
#15079=CARTESIAN_POINT('',(-0.0279999999166667,-0.00764161763054874,-0.0204554035689891));
#15080=CARTESIAN_POINT('',(-0.0270000000833333,-0.00764161763054874,-0.0204554035689891));
#15081=CARTESIAN_POINT('',(-0.02600000025,-0.00764161763054874,-0.0204554035689891));
#15082=CARTESIAN_POINT('',(-0.0275,-0.006003117026,-0.018816902965));
#15083=CARTESIAN_POINT('',(-0.0275,-0.0132943574755,-0.0146073033285));
#15084=CARTESIAN_POINT('',(-0.026000000125,-0.013894090321,-0.016845536779));
#15085=CARTESIAN_POINT('',(-0.0270000000833333,-0.013894090321,-0.016845536779));
#15086=CARTESIAN_POINT('',(-0.0280000000416667,-0.013894090321,-0.016845536779));
#15087=CARTESIAN_POINT('',(-0.029,-0.013894090321,-0.016845536779));
#15088=CARTESIAN_POINT('',(-0.019,-0.01534297906,-0.016457308211));
#15089=CARTESIAN_POINT('',(-0.02899999975,-0.0163658443303253,-0.017554462092077));
#15090=CARTESIAN_POINT('',(-0.0279999999166667,-0.0163658443303253,-0.017554462092077));
#15091=CARTESIAN_POINT('',(-0.0270000000833333,-0.0163658443303253,-0.017554462092077));
#15092=CARTESIAN_POINT('',(-0.02600000025,-0.0163658443303253,-0.017554462092077));
#15093=CARTESIAN_POINT('',(-0.019,0.,0.));
#15094=CARTESIAN_POINT('',(-0.02899999975,-0.0233855322854857,-0.00539600590478796));
#15095=CARTESIAN_POINT('',(-0.0279999999166667,-0.0233855322854857,-0.00539600590478796));
#15096=CARTESIAN_POINT('',(-0.0270000000833333,-0.0233855322854857,-0.00539600590478796));
#15097=CARTESIAN_POINT('',(-0.02600000025,-0.0233855322854857,-0.00539600590478796));
#15098=CARTESIAN_POINT('',(-0.019,-0.021923936519,-0.00505875553));
#15099=CARTESIAN_POINT('',(-0.02899999975,-0.0215357079510552,-0.00360986679064437));
#15100=CARTESIAN_POINT('',(-0.0279999999166667,-0.0215357079510552,-0.00360986679064437));
#15101=CARTESIAN_POINT('',(-0.0270000000833333,-0.0215357079510552,-0.00360986679064437));
#15102=CARTESIAN_POINT('',(-0.02600000025,-0.0215357079510552,-0.00360986679064437));
#15103=CARTESIAN_POINT('',(-0.0275,-0.019297474501,-0.00420959963649999));
#15104=CARTESIAN_POINT('',(-0.0275,-0.019297474501,0.00420959963649999));
#15105=CARTESIAN_POINT('',(-0.026000000125,-0.021535707951,0.00360986679099999));
#15106=CARTESIAN_POINT('',(-0.0270000000833333,-0.021535707951,0.00360986679099999));
#15107=CARTESIAN_POINT('',(-0.0280000000416667,-0.021535707951,0.00360986679099999));
#15108=CARTESIAN_POINT('',(-0.029,-0.021535707951,0.00360986679099999));
#15109=CARTESIAN_POINT('',(-0.019,-0.021923936519,0.00505875553));
#15110=CARTESIAN_POINT('',(-0.02899999975,-0.0233855322867651,0.00539600589938632));
#15111=CARTESIAN_POINT('',(-0.0279999999166667,-0.0233855322867651,0.00539600589938632));
#15112=CARTESIAN_POINT('',(-0.0270000000833333,-0.0233855322867651,0.00539600589938632));
#15113=CARTESIAN_POINT('',(-0.02600000025,-0.0233855322867651,0.00539600589938632));
#15114=CARTESIAN_POINT('',(-0.019,0.,0.));
#15115=CARTESIAN_POINT('',(-0.02899999975,-0.0163658443387112,0.0175544620846403));
#15116=CARTESIAN_POINT('',(-0.0279999999166667,-0.0163658443387112,0.0175544620846403));
#15117=CARTESIAN_POINT('',(-0.0270000000833333,-0.0163658443387112,0.0175544620846403));
#15118=CARTESIAN_POINT('',(-0.02600000025,-0.0163658443387112,0.0175544620846403));
#15119=CARTESIAN_POINT('',(-0.019,-0.01534297906,0.016457308211));
#15120=CARTESIAN_POINT('',(-0.02899999975,-0.0138940903205647,0.0168455367786476));
#15121=CARTESIAN_POINT('',(-0.0279999999166667,-0.0138940903205647,0.0168455367786476));
#15122=CARTESIAN_POINT('',(-0.0270000000833333,-0.0138940903205647,0.0168455367786476));
#15123=CARTESIAN_POINT('',(-0.02600000025,-0.0138940903205647,0.0168455367786476));
#15124=CARTESIAN_POINT('',(-0.0275,-0.0132943574755,0.0146073033285));
#15125=CARTESIAN_POINT('',(-0.0275,-0.006003117026,0.018816902965));
#15126=CARTESIAN_POINT('',(-0.026000000125,-0.007641617631,0.02045540357));
#15127=CARTESIAN_POINT('',(-0.0270000000833333,-0.007641617631,0.02045540357));
#15128=CARTESIAN_POINT('',(-0.0280000000416667,-0.007641617631,0.02045540357));
#15129=CARTESIAN_POINT('',(-0.029,-0.007641617631,0.02045540357));
#15130=CARTESIAN_POINT('',(-0.019,-0.006580957459,0.021516063741));
#15131=CARTESIAN_POINT('',(-0.02899999975,-0.0070196879558403,0.0229504679905553));
#15132=CARTESIAN_POINT('',(-0.0279999999166667,-0.0070196879558403,0.0229504679905553));
#15133=CARTESIAN_POINT('',(-0.0270000000833333,-0.0070196879558403,0.0229504679905553));
#15134=CARTESIAN_POINT('',(-0.02600000025,-0.0070196879558403,0.0229504679905553));
#15135=CARTESIAN_POINT('',(-0.019,0.,0.));
#15136=CARTESIAN_POINT('',(-0.02899999975,0.00701968794532321,0.0229504679941452));
#15137=CARTESIAN_POINT('',(-0.0279999999166667,0.00701968794532321,0.0229504679941452));
#15138=CARTESIAN_POINT('',(-0.0270000000833333,0.00701968794532321,0.0229504679941452));
#15139=CARTESIAN_POINT('',(-0.02600000025,0.00701968794532321,0.0229504679941452));
#15140=CARTESIAN_POINT('',(-0.019,0.006580957459,0.021516063741));
#15141=CARTESIAN_POINT('',(-0.02899999975,0.00764161763098383,0.0204554035694242));
#15142=CARTESIAN_POINT('',(-0.0279999999166667,0.00764161763098383,0.0204554035694242));
#15143=CARTESIAN_POINT('',(-0.0270000000833333,0.00764161763098383,0.0204554035694242));
#15144=CARTESIAN_POINT('',(-0.02600000025,0.00764161763098383,0.0204554035694242));
#15145=CARTESIAN_POINT('',(-0.0275,0.006003117026,0.018816902965));
#15146=CARTESIAN_POINT('',(-0.0269999999999846,-1.36038104775004E-13,2.6489787551435E-18));
#15147=CARTESIAN_POINT('',(-0.0269999999998682,1.36039743730353E-13,-2.59930748974073E-18));
#15148=CARTESIAN_POINT('',(-0.0270000001246841,-6.97351005096951E-12,-0.0339999999999195));
#15149=CARTESIAN_POINT('',(-0.0270000001249341,-1.94544521920252E-11,0.0339999999999195));
#15150=CARTESIAN_POINT('',(-0.0269999999998682,-1.94544562196518E-11,0.0339999999998389));
#15151=CARTESIAN_POINT('',(-0.0269999999998739,-0.00445058961092908,0.0339999999973102));
#15152=CARTESIAN_POINT('',(-0.0269999999998853,-0.01334969402564,0.0322296836269298));
#15153=CARTESIAN_POINT('',(-0.0269999999998997,-0.0246676067857547,0.0246675319043401));
#15154=CARTESIAN_POINT('',(-0.0269999999999094,-0.0322296622477484,0.0133499720628638));
#15155=CARTESIAN_POINT('',(-0.0269999999999128,-0.0348851688773134,-6.40291627412936E-12));
#15156=CARTESIAN_POINT('',(-0.0269999999999094,-0.0322296622428478,-0.0133499720746949));
#15157=CARTESIAN_POINT('',(-0.0269999999998997,-0.0246676067766996,-0.0246675319133952));
#15158=CARTESIAN_POINT('',(-0.0269999999998853,-0.0133496940138089,-0.0322296836318303));
#15159=CARTESIAN_POINT('',(-0.0269999999998739,-0.00445058959844815,-0.0339999999989439));
#15160=CARTESIAN_POINT('',(-0.0269999999998682,-6.97352071331679E-12,-0.0339999999998389));
#15161=CARTESIAN_POINT('',(-0.087860759494,0.,0.));
#15162=CARTESIAN_POINT('',(-0.0448,0.,0.));
#15163=CARTESIAN_POINT('',(-0.0448000003749039,-1.43991482401222E-12,0.0160358983848022));
#15164=CARTESIAN_POINT('',(-0.044799999999904,-9.30247185607308E-12,-0.0160358983848022));
#15165=CARTESIAN_POINT('',(-0.0448,-6.88880368742238E-12,0.016035898385));
#15166=CARTESIAN_POINT('',(-0.0448,-0.00209909419616183,0.0160358983840983));
#15167=CARTESIAN_POINT('',(-0.0448,-0.00629630402268758,0.0152009391664744));
#15168=CARTESIAN_POINT('',(-0.0448,-0.0116343304626057,0.0116342951503842));
#15169=CARTESIAN_POINT('',(-0.0448,-0.0152009290802918,0.00629643516400925));
#15170=CARTESIAN_POINT('',(-0.0448,-0.0164533830369911,1.89724333662342E-12));
#15171=CARTESIAN_POINT('',(-0.0448,-0.0152009290817439,-0.0062964351605036));
#15172=CARTESIAN_POINT('',(-0.0448,-0.0116343304652888,-0.0116342951477011));
#15173=CARTESIAN_POINT('',(-0.0448,-0.00629630402619322,-0.0152009391650224));
#15174=CARTESIAN_POINT('',(-0.0448,-0.00209909419986004,-0.0160358983836142));
#15175=CARTESIAN_POINT('',(-0.0448,-1.0587010404128E-11,-0.016035898385));
#15176=CARTESIAN_POINT('',(-0.0292999999998881,3.50882717550253E-13,-3.61538547232193E-19));
#15177=CARTESIAN_POINT('',(-0.0293,0.,1.29739916218158E-17));
#15178=CARTESIAN_POINT('',(-0.0293000001249039,-4.18441562143595E-12,0.0160358983848022));
#15179=CARTESIAN_POINT('',(-0.0293000001249039,-5.46894785937705E-12,-0.0160358983848022));
#15180=CARTESIAN_POINT('',(-0.0292999999998079,-5.46895656244816E-12,-0.0160358983846046));
#15181=CARTESIAN_POINT('',(-0.0292999999998007,-0.00209909419504539,-0.0160358983839346));
#15182=CARTESIAN_POINT('',(-0.0292999999997864,-0.00629630402226934,-0.0152009391665087));
#15183=CARTESIAN_POINT('',(-0.0292999999997682,-0.0116343304630323,-0.0116342951499371));
#15184=CARTESIAN_POINT('',(-0.0292999999997561,-0.0152009290809598,-0.00629643516255718));
#15185=CARTESIAN_POINT('',(-0.0292999999997518,-0.0164533830370793,6.59004884789626E-13));
#15186=CARTESIAN_POINT('',(-0.0292999999997561,-0.0152009290804555,0.00629643516377478));
#15187=CARTESIAN_POINT('',(-0.0292999999997682,-0.0116343304621004,0.011634295150869));
#15188=CARTESIAN_POINT('',(-0.0292999999997864,-0.0062963040210517,0.015200939167013));
#15189=CARTESIAN_POINT('',(-0.0292999999998007,-0.00209909419376085,0.0160358983841027));
#15190=CARTESIAN_POINT('',(-0.0292999999998079,-4.18441069673782E-12,0.0160358983846046));
#15191=CARTESIAN_POINT('',(-0.0280000000000153,-1.36039948891632E-13,2.12798109529093E-18));
#15192=CARTESIAN_POINT('',(-0.0280000000001317,1.36035990293993E-13,-2.40331363620194E-18));
#15193=CARTESIAN_POINT('',(-0.0279999998753159,-3.05296983152609E-12,0.0339999999999195));
#15194=CARTESIAN_POINT('',(-0.0279999998750659,-2.53352639798974E-11,-0.0339999999999195));
#15195=CARTESIAN_POINT('',(-0.0280000000001317,-2.53352755643033E-11,-0.033999999999839));
#15196=CARTESIAN_POINT('',(-0.0280000000001261,-0.00445058961672823,-0.0339999999965404));
#15197=CARTESIAN_POINT('',(-0.0280000000001147,-0.0133496940309697,-0.0322296836246866));
#15198=CARTESIAN_POINT('',(-0.0280000000001003,-0.0246676067896425,-0.0246675319004057));
#15199=CARTESIAN_POINT('',(-0.0280000000000906,-0.0322296622497385,-0.0133499720579734));
#15200=CARTESIAN_POINT('',(-0.0280000000000872,-0.0348851688772805,1.14312184329868E-11));
#15201=CARTESIAN_POINT('',(-0.0280000000000906,-0.0322296622409894,0.0133499720790955));
#15202=CARTESIAN_POINT('',(-0.0280000000001003,-0.0246676067734763,0.0246675319165719));
#15203=CARTESIAN_POINT('',(-0.0280000000001147,-0.0133496940098477,0.0322296836334355));
#15204=CARTESIAN_POINT('',(-0.0280000000001261,-0.00445058959444593,0.0339999999994571));
#15205=CARTESIAN_POINT('',(-0.0280000000001317,-3.05298233072731E-12,0.033999999999839));
#15206=CARTESIAN_POINT('',(-0.087860759494,0.,0.));
#15207=CARTESIAN_POINT('',(-0.0447999999998881,-3.50878864290858E-13,1.27902351783967E-19));
#15208=CARTESIAN_POINT('',(-0.0444999999996631,-3.49856951876166E-13,6.65098269064164E-20));
#15209=CARTESIAN_POINT('',(-0.0444999999997187,0.016335898384458,6.65098269064164E-20));
#15210=CARTESIAN_POINT('',(-0.087860759494,0.,2.74627544186333E-49));
#15211=CARTESIAN_POINT('',(-0.033133974596,0.,1.21245840199241E-17));
#15212=CARTESIAN_POINT('',(-0.0331339745961753,-9.30247461674151E-12,-0.01603589838493));
#15213=CARTESIAN_POINT('',(-0.033133974471,-7.45337677166523E-12,0.016035898385));
#15214=CARTESIAN_POINT('',(-0.033133974596,-1.0587010404128E-11,-0.016035898385));
#15215=CARTESIAN_POINT('',(-0.033133974596,-0.00209909419983651,-0.0160358983836142));
#15216=CARTESIAN_POINT('',(-0.033133974596,-0.0062963040261227,-0.0152009391650413));
#15217=CARTESIAN_POINT('',(-0.033133974596,-0.0116343304651797,-0.0116342951477968));
#15218=CARTESIAN_POINT('',(-0.033133974596,-0.015200929081652,-0.00629643516070066));
#15219=CARTESIAN_POINT('',(-0.033133974596,-0.0164533830369816,1.60761173666999E-12));
#15220=CARTESIAN_POINT('',(-0.033133974596,-0.0152009290804216,0.00629643516367116));
#15221=CARTESIAN_POINT('',(-0.033133974596,-0.0116343304629062,0.0116342951500703));
#15222=CARTESIAN_POINT('',(-0.033133974596,-0.00629630402315223,0.0152009391662717));
#15223=CARTESIAN_POINT('',(-0.033133974596,-0.00209909419670289,0.0160358983840244));
#15224=CARTESIAN_POINT('',(-0.033133974596,-7.45338585686584E-12,0.016035898385));
#15225=CARTESIAN_POINT('',(-0.0445,3.78301144317866E-6,1.64798730217797E-19));
#15226=CARTESIAN_POINT('',(-0.0445,0.,0.));
#15227=CARTESIAN_POINT('',(-0.0445,-0.0119306429063121,0.0114497029323385));
#15228=CARTESIAN_POINT('',(-0.044499999875,-0.0158810549881622,0.00460738839930129));
#15229=CARTESIAN_POINT('',(-0.0445,-0.013988882352324,0.0191311570514775));
#15230=CARTESIAN_POINT('',(-0.0445,-0.0133028025302656,0.016570672323168));
#15231=CARTESIAN_POINT('',(-0.0445,-0.0126167227082072,0.0140101875948586));
#15232=CARTESIAN_POINT('',(-0.0445,-0.0119306428861488,0.0114497028665492));
#15233=CARTESIAN_POINT('',(-0.0445000000004407,-0.01398888233812,0.0191311570560501));
#15234=CARTESIAN_POINT('',(-0.0445000000054389,-1.31298894547398E-11,2.57689317088404E-11));
#15235=CARTESIAN_POINT('',(-0.044500000000146,-0.00957362679562088,0.021680305939673));
#15236=CARTESIAN_POINT('',(-0.0445,-0.00395041209800161,0.0160570912714795));
#15237=CARTESIAN_POINT('',(-0.0445,-0.00582481702234961,0.0179314961816983));
#15238=CARTESIAN_POINT('',(-0.0445,-0.0076992219466976,0.019805901091917));
#15239=CARTESIAN_POINT('',(-0.0445,-0.0095736268710456,0.0216803060021358));
#15240=CARTESIAN_POINT('',(-0.044499999875,-0.00395041209657952,0.0160570912579534));
#15241=CARTESIAN_POINT('',(-0.0445,0.,0.));
#15242=CARTESIAN_POINT('',(-0.0444999998749998,0.00395041214632822,0.0160570913147367));
#15243=CARTESIAN_POINT('',(-0.0445,0.00957362687104559,0.0216803060021358));
#15244=CARTESIAN_POINT('',(-0.0445,0.00769922196196155,0.019805901107181));
#15245=CARTESIAN_POINT('',(-0.0445,0.00582481705287752,0.0179314962122262));
#15246=CARTESIAN_POINT('',(-0.0445,0.00395041214379348,0.0160570913172714));
#15247=CARTESIAN_POINT('',(-0.0445000000002923,0.00957362684875627,0.0216803060057704));
#15248=CARTESIAN_POINT('',(-0.0445000000054388,1.31301128770511E-11,2.57694144345576E-11));
#15249=CARTESIAN_POINT('',(-0.0445000000002202,0.0139888823212884,0.0191311569644422));
#15250=CARTESIAN_POINT('',(-0.0445,0.0119306428861488,0.0114497028665492));
#15251=CARTESIAN_POINT('',(-0.0445,0.0126167227082072,0.0140101875948586));
#15252=CARTESIAN_POINT('',(-0.0445,0.0133028025302656,0.016570672323168));
#15253=CARTESIAN_POINT('',(-0.0445,0.013988882352324,0.0191311570514775));
#15254=CARTESIAN_POINT('',(-0.0445,0.0119306428918697,0.0114497028601498));
#15255=CARTESIAN_POINT('',(-0.0445,0.,0.));
#15256=CARTESIAN_POINT('',(-0.0444999999996452,0.0159746110500761,0.00427173727880919));
#15257=CARTESIAN_POINT('',(-0.0445,0.0235948629797496,0.00222989690610838));
#15258=CARTESIAN_POINT('',(-0.0445,0.0210547789802328,0.00291051037320731));
#15259=CARTESIAN_POINT('',(-0.0445,0.018514694980716,0.00359112384030625));
#15260=CARTESIAN_POINT('',(-0.0445,0.0159746109811992,0.00427173730740518));
#15261=CARTESIAN_POINT('',(-0.0445000000001154,0.0235948629947594,0.0022298969152439));
#15262=CARTESIAN_POINT('',(-0.0445000000068876,4.40842231272297E-11,8.49853498151601E-13));
#15263=CARTESIAN_POINT('',(-0.0445000000001778,0.0235625090884613,-0.00254914897306764));
#15264=CARTESIAN_POINT('',(-0.0445,0.0158810549909967,-0.00460738840309584));
#15265=CARTESIAN_POINT('',(-0.0445,0.0184415397191314,-0.00392130858560222));
#15266=CARTESIAN_POINT('',(-0.0445,0.0210020244472661,-0.0032352287681086));
#15267=CARTESIAN_POINT('',(-0.0445,0.0235625091754008,-0.00254914895061497));
#15268=CARTESIAN_POINT('',(-0.044499999875,0.0158810549891071,-0.00460738839604404));
#15269=CARTESIAN_POINT('',(-0.0445,0.,0.));
#15270=CARTESIAN_POINT('',(-0.0444999998749998,0.0119306429043919,-0.0114497029343883));
#15271=CARTESIAN_POINT('',(-0.0445,0.013988882352324,-0.0191311570514775));
#15272=CARTESIAN_POINT('',(-0.0445,0.0133028025363262,-0.0165706723457866));
#15273=CARTESIAN_POINT('',(-0.0445,0.0126167227203284,-0.0140101876400956));
#15274=CARTESIAN_POINT('',(-0.0445,0.0119306429043306,-0.0114497029344047));
#15275=CARTESIAN_POINT('',(-0.0445000000004407,0.01398888233812,-0.0191311570560501));
#15276=CARTESIAN_POINT('',(-0.0445000000054393,1.31303038846426E-11,-2.57695957250192E-11));
#15277=CARTESIAN_POINT('',(-0.044500000000146,0.00957362679562087,-0.021680305939673));
#15278=CARTESIAN_POINT('',(-0.0445,0.00395041209800159,-0.0160570912714795));
#15279=CARTESIAN_POINT('',(-0.0445,0.00582481702234959,-0.0179314961816983));
#15280=CARTESIAN_POINT('',(-0.0445,0.00769922194669759,-0.019805901091917));
#15281=CARTESIAN_POINT('',(-0.0445,0.00957362687104559,-0.0216803060021358));
#15282=CARTESIAN_POINT('',(-0.044499999875,0.00395041209972926,-0.0160570912569995));
#15283=CARTESIAN_POINT('',(-0.0445,0.,0.));
#15284=CARTESIAN_POINT('',(-0.0444999998749998,-0.00395041214962159,-0.0160570913139264));
#15285=CARTESIAN_POINT('',(-0.0445,-0.0095736268710456,-0.0216803060021358));
#15286=CARTESIAN_POINT('',(-0.0445,-0.00769922196237542,-0.0198059011075949));
#15287=CARTESIAN_POINT('',(-0.0445,-0.00582481705370523,-0.0179314962130539));
#15288=CARTESIAN_POINT('',(-0.0445,-0.00395041214503505,-0.016057091318513));
#15289=CARTESIAN_POINT('',(-0.0445000000002922,-0.00957362684875627,-0.0216803060057704));
#15290=CARTESIAN_POINT('',(-0.0445000000054376,-1.31302623148723E-11,-2.57695601066413E-11));
#15291=CARTESIAN_POINT('',(-0.0445000000002202,-0.0139888823212884,-0.0191311569644422));
#15292=CARTESIAN_POINT('',(-0.0445,-0.0119306428861488,-0.0114497028665492));
#15293=CARTESIAN_POINT('',(-0.0445,-0.0126167227082072,-0.0140101875948586));
#15294=CARTESIAN_POINT('',(-0.0445,-0.0133028025302656,-0.016570672323168));
#15295=CARTESIAN_POINT('',(-0.0445,-0.013988882352324,-0.0191311570514775));
#15296=CARTESIAN_POINT('',(-0.044499999875,-0.0119306428942181,-0.0114497028577028));
#15297=CARTESIAN_POINT('',(-0.0445,0.,0.));
#15298=CARTESIAN_POINT('',(-0.0444999998749998,-0.0158810550546861,-0.00460738838227197));
#15299=CARTESIAN_POINT('',(-0.0445,-0.0235625091754008,-0.00254914895061497));
#15300=CARTESIAN_POINT('',(-0.0445,-0.0210020244688091,-0.00323522876233617));
#15301=CARTESIAN_POINT('',(-0.0445,-0.0184415397622174,-0.00392130857405737));
#15302=CARTESIAN_POINT('',(-0.0445,-0.0158810550556257,-0.00460738838577856));
#15303=CARTESIAN_POINT('',(-0.0445000000003707,-0.0235625091821229,-0.00254914894712841));
#15304=CARTESIAN_POINT('',(-0.0445000000057756,-1.48440606719702E-11,1.19635928943991E-17));
#15305=CARTESIAN_POINT('',(-0.0445000000001852,-0.023562509088512,0.00254914897305407));
#15306=CARTESIAN_POINT('',(-0.0445,-0.0158810549893007,0.00460738840355029));
#15307=CARTESIAN_POINT('',(-0.0445,-0.0184415397180007,0.00392130858590519));
#15308=CARTESIAN_POINT('',(-0.0445,-0.0210020244467008,0.00323522876826008));
#15309=CARTESIAN_POINT('',(-0.0445,-0.0235625091754008,0.00254914895061497));
#15310=CARTESIAN_POINT('',(-0.0445000000003622,-0.01,-0.0173205080756646));
#15311=CARTESIAN_POINT('',(-0.044500000000308,-0.01,-0.0197705080752687));
#15312=CARTESIAN_POINT('',(-0.044500000000337,-0.0200000000003441,2.58823356637625E-19));
#15313=CARTESIAN_POINT('',(-0.044500000000337,-0.02,-0.00244999999980786));
#15314=CARTESIAN_POINT('',(-0.0445000000003614,-0.0200000000006125,0.00244999999974705));
#15315=CARTESIAN_POINT('',(-0.044500000000337,-0.0199999999996559,-5.49576725493911E-20));
#15316=CARTESIAN_POINT('',(-0.0445000000003622,-0.01,0.0173205080756646));
#15317=CARTESIAN_POINT('',(-0.0445000000004165,-0.01,0.0148705080755215));
#15318=CARTESIAN_POINT('',(-0.0445000000003622,0.01,0.0173205080756646));
#15319=CARTESIAN_POINT('',(-0.0445000000004165,0.01,0.0148705080755215));
#15320=CARTESIAN_POINT('',(-0.044500000000337,0.0199999999996559,9.70768175342268E-20));
#15321=CARTESIAN_POINT('',(-0.044500000000337,0.02,-0.00244999999980786));
#15322=CARTESIAN_POINT('',(-0.0445000000003614,0.0199999999993875,0.00244999999974705));
#15323=CARTESIAN_POINT('',(-0.044500000000337,0.0200000000003441,-3.39924582891466E-19));
#15324=CARTESIAN_POINT('',(-0.0445000000003622,0.01,-0.0173205080756646));
#15325=CARTESIAN_POINT('',(-0.044500000000308,0.01,-0.0197705080752687));
#15326=CARTESIAN_POINT('',(-0.0331339745963505,2.10159751068267E-14,-6.83211248137564E-19));
#15327=CARTESIAN_POINT('',(-0.0331339745963505,1.9700566598701E-15,-0.0175358983853182));
#15328=CARTESIAN_POINT('',(-0.0342520085854507,-2.75308153152585E-18,-0.0165358983850228));
#15329=CARTESIAN_POINT('',(-0.0342520085854131,0.0039504121119975,-0.0160570912542433));
#15330=CARTESIAN_POINT('',(-0.0342520085854251,0.00265925059751097,-0.0163747465508529));
#15331=CARTESIAN_POINT('',(-0.0342520085854379,0.0013296627181151,-0.0165358983850421));
#15332=CARTESIAN_POINT('',(-0.0342520085854507,2.21354587678372E-17,-0.0165358983850228));
#15333=CARTESIAN_POINT('',(-0.0342520089022404,0.00395041215716228,-0.0160570913151623));
#15334=CARTESIAN_POINT('',(-0.034433013025824,0.00415647342831627,-0.0162631525862801));
#15335=CARTESIAN_POINT('',(-0.0343819209654274,0.00408372706329651,-0.0161904062212731));
#15336=CARTESIAN_POINT('',(-0.0343218321493816,0.00401493175248625,-0.0161216109104749));
#15337=CARTESIAN_POINT('',(-0.0342520087109173,0.00395041221532456,-0.0160570913733245));
#15338=CARTESIAN_POINT('',(-0.0344330128635322,0.00415647320725126,-0.0162631523535427));
#15339=CARTESIAN_POINT('',(-0.0344330127020119,0.0120060661714172,-0.0117311874792547));
#15340=CARTESIAN_POINT('',(-0.0344330127020133,0.00986802652236389,-0.0139193244899128));
#15341=CARTESIAN_POINT('',(-0.034433012702027,0.00712047520748447,-0.0155056239641693));
#15342=CARTESIAN_POINT('',(-0.0344330127020451,0.00415647313777669,-0.0162631520817075));
#15343=CARTESIAN_POINT('',(-0.0344330130235902,0.0120060665703178,-0.0117311878690224));
#15344=CARTESIAN_POINT('',(-0.0342520086858872,0.0119306429240885,-0.0114497029892201));
#15345=CARTESIAN_POINT('',(-0.0343218322133286,0.0119542587426544,-0.0115378384239647));
#15346=CARTESIAN_POINT('',(-0.0343819208998164,0.0119794395195841,-0.0116318143628348));
#15347=CARTESIAN_POINT('',(-0.0344330130239393,0.0120060665702831,-0.0117311878688929));
#15348=CARTESIAN_POINT('',(-0.0342520087102053,0.01193064288788,-0.0114497028645091));
#15349=CARTESIAN_POINT('',(-0.0342520085854456,0.0158810549917541,-0.00460738838842381));
#15350=CARTESIAN_POINT('',(-0.0342520085854222,0.0151400885910336,-0.00716140102293671));
#15351=CARTESIAN_POINT('',(-0.0342520085854116,0.0137719995116387,-0.00953100081866742));
#15352=CARTESIAN_POINT('',(-0.0342520085854105,0.0119306428896003,-0.0114497028629186));
#15353=CARTESIAN_POINT('',(-0.0342520089017979,0.015881055068089,-0.00460738837380816));
#15354=CARTESIAN_POINT('',(-0.0344330129938737,0.0161625399379626,-0.00453196473023928));
#15355=CARTESIAN_POINT('',(-0.034381920935403,0.016063166568659,-0.00455859174429499));
#15356=CARTESIAN_POINT('',(-0.0343218321405072,0.0159691904637724,-0.00458377256570873));
#15357=CARTESIAN_POINT('',(-0.0342520087100322,0.0158810551471781,-0.00460738835261631));
#15358=CARTESIAN_POINT('',(-0.0344330128473697,0.0161625396544538,-0.00453196480620524));
#15359=CARTESIAN_POINT('',(-0.0344330127014593,0.,-9.36178073300934E-16));
#15360=CARTESIAN_POINT('',(-0.0344330129926893,0.0161625399363783,0.00453196473066377));
#15361=CARTESIAN_POINT('',(-0.0342520086857044,0.0158810551164701,0.00460738836084449));
#15362=CARTESIAN_POINT('',(-0.034321832199017,0.0159691905333651,0.00458377254706142));
#15363=CARTESIAN_POINT('',(-0.034381920878985,0.0160631664582187,0.00455859177388738));
#15364=CARTESIAN_POINT('',(-0.0344330129962152,0.0161625399425169,0.00453196472901897));
#15365=CARTESIAN_POINT('',(-0.0342520087102228,0.0158810549894791,0.0046073883955136));
#15366=CARTESIAN_POINT('',(-0.0342520085854105,0.0119306428896003,0.0114497028629186));
#15367=CARTESIAN_POINT('',(-0.0342520085854116,0.0137719995099208,0.00953100082045744));
#15368=CARTESIAN_POINT('',(-0.0342520085854222,0.0151400885885014,0.00716140102736863));
#15369=CARTESIAN_POINT('',(-0.0342520085854456,0.0158810549896802,0.00460738839557196));
#15370=CARTESIAN_POINT('',(-0.034252008901483,0.0119306429110209,0.0114497029404512));
#15371=CARTESIAN_POINT('',(-0.034433013023346,0.0120060665704802,0.0117311878682453));
#15372=CARTESIAN_POINT('',(-0.0343819209636497,0.0119794395533804,0.0116318144875807));
#15373=CARTESIAN_POINT('',(-0.034321832146695,0.0119542587212213,0.0115378383439753));
#15374=CARTESIAN_POINT('',(-0.0342520087094024,0.0119306429320419,0.0114497030189024));
#15375=CARTESIAN_POINT('',(-0.0344330128624694,0.0120060664878914,0.0117311875540647));
#15376=CARTESIAN_POINT('',(-0.0344330127020451,0.00415647328920086,0.0162631520430071));
#15377=CARTESIAN_POINT('',(-0.034433012702027,0.00712047535552922,0.0155056238969325));
#15378=CARTESIAN_POINT('',(-0.0344330127020133,0.00986802665874799,0.0139193243940575));
#15379=CARTESIAN_POINT('',(-0.0344330127020119,0.012006066288595,0.0117311873593312));
#15380=CARTESIAN_POINT('',(-0.0344330130250702,0.00415647342795653,0.0162631525859204));
#15381=CARTESIAN_POINT('',(-0.0342520086868176,0.00395041219305555,0.0160570913510556));
#15382=CARTESIAN_POINT('',(-0.0343218322145698,0.00401493180963198,0.0161216109676207));
#15383=CARTESIAN_POINT('',(-0.0343819209012451,0.00408372697198972,0.0161904061299663));
#15384=CARTESIAN_POINT('',(-0.0344330130254722,0.00415647342781538,0.0162631525857792));
#15385=CARTESIAN_POINT('',(-0.0342520087102066,0.00395041210349994,0.0160570912562923));
#15386=CARTESIAN_POINT('',(-0.0342520085854507,-3.62334336342478E-17,0.0165358983850228));
#15387=CARTESIAN_POINT('',(-0.0342520085854379,0.00132966271520138,0.0165358983850421));
#15388=CARTESIAN_POINT('',(-0.0342520085854251,0.00265925059168442,0.0163747465515626));
#15389=CARTESIAN_POINT('',(-0.0342520085854131,0.00395041210350958,0.0160570912563315));
#15390=CARTESIAN_POINT('',(-0.0342520087102254,-1.48481175253027E-12,0.0165358983850114));
#15391=CARTESIAN_POINT('',(-0.0331339745963505,2.52979239737867E-14,0.0175358983853182));
#15392=CARTESIAN_POINT('',(-0.0331339745963505,-2.10154316653151E-14,8.38648712071716E-19));
#15393=CARTESIAN_POINT('',(-0.0342520086872413,-0.00395041219344707,-0.0160570913514471));
#15394=CARTESIAN_POINT('',(-0.0343218322149425,-0.00401493181003064,-0.0161216109680193));
#15395=CARTESIAN_POINT('',(-0.0343819209015701,-0.00408372697239052,-0.0161904061303671));
#15396=CARTESIAN_POINT('',(-0.0344330130257521,-0.00415647342821389,-0.0162631525861777));
#15397=CARTESIAN_POINT('',(-0.0342520087102066,-0.00395041210679331,-0.0160570912554821));
#15398=CARTESIAN_POINT('',(-0.0344330130253497,-0.0041564734283552,-0.016263152586319));
#15399=CARTESIAN_POINT('',(-0.0342520085854507,-1.29547937350208E-17,-0.0165358983850228));
#15400=CARTESIAN_POINT('',(-0.0342520085854379,-0.00132966271633194,-0.0165358983850421));
#15401=CARTESIAN_POINT('',(-0.0342520085854251,-0.00265925059394516,-0.0163747465512872));
#15402=CARTESIAN_POINT('',(-0.0342520085854131,-0.00395041210680295,-0.0160570912555213));
#15403=CARTESIAN_POINT('',(-0.0342520085854131,-0.00395041211199747,0.0160570912542433));
#15404=CARTESIAN_POINT('',(-0.0342520085854251,-0.00265925059799155,0.0163747465507347));
#15405=CARTESIAN_POINT('',(-0.0342520085854379,-0.00132966271910495,0.0165358983849227));
#15406=CARTESIAN_POINT('',(-0.0342520085854507,-1.48481417980218E-12,0.0165358983850228));
#15407=CARTESIAN_POINT('',(-0.0342520089022404,-0.00395041215716228,0.0160570913151623));
#15408=CARTESIAN_POINT('',(-0.0344330130255441,-0.00415647342791775,0.0162631525858816));
#15409=CARTESIAN_POINT('',(-0.0343819209651601,-0.00408372706297781,0.0161904062209545));
#15410=CARTESIAN_POINT('',(-0.0343218321493167,-0.00401493175242626,0.0161216109104149));
#15411=CARTESIAN_POINT('',(-0.0342520087109173,-0.00395041221532456,0.0160570913733245));
#15412=CARTESIAN_POINT('',(-0.0344330128633927,-0.00415647320705185,0.0162631523533433));
#15413=CARTESIAN_POINT('',(-0.0344330127020119,-0.0120060661717061,0.011731187478959));
#15414=CARTESIAN_POINT('',(-0.0344330127020133,-0.00986802652257684,0.0139193244898027));
#15415=CARTESIAN_POINT('',(-0.034433012702027,-0.00712047520753155,0.0155056239641843));
#15416=CARTESIAN_POINT('',(-0.0344330127020451,-0.00415647313763734,0.0162631520817431));
#15417=CARTESIAN_POINT('',(-0.0344330130231881,-0.012006066570108,0.0117311878682395));
#15418=CARTESIAN_POINT('',(-0.0342520087094023,-0.0119306429320419,0.0114497030189024));
#15419=CARTESIAN_POINT('',(-0.0343218322266828,-0.0119542587482748,0.0115378384449406));
#15420=CARTESIAN_POINT('',(-0.0343819209052242,-0.0119794395224397,0.0116318143734919));
#15421=CARTESIAN_POINT('',(-0.03443301302348,-0.0120060665700438,0.0117311878679997));
#15422=CARTESIAN_POINT('',(-0.034252008839487,-0.0119306428898001,0.0114497028624593));
#15423=CARTESIAN_POINT('',(-0.0342520085854456,-0.0158810549917541,0.00460738838842376));
#15424=CARTESIAN_POINT('',(-0.0342520085854222,-0.0151400885910772,0.0071614010227863));
#15425=CARTESIAN_POINT('',(-0.0342520085854116,-0.013771999511801,0.00953100081838915));
#15426=CARTESIAN_POINT('',(-0.0342520085854105,-0.0119306428899256,0.0114497028625797));
#15427=CARTESIAN_POINT('',(-0.0342520089017979,-0.015881055068089,0.00460738837380815));
#15428=CARTESIAN_POINT('',(-0.0344330130210024,-0.016162539995109,0.00453196471727475));
#15429=CARTESIAN_POINT('',(-0.0343819209617668,-0.0160631666155137,0.00455859173408813));
#15430=CARTESIAN_POINT('',(-0.0343218321465883,-0.0159691904714484,0.00458377256365195));
#15431=CARTESIAN_POINT('',(-0.0342520087100322,-0.0158810551471781,0.00460738835261631));
#15432=CARTESIAN_POINT('',(-0.034433012862003,-0.0161625396803212,0.00453196480545577));
#15433=CARTESIAN_POINT('',(-0.034433012702032,-0.0161625394592827,-0.00453196456511526));
#15434=CARTESIAN_POINT('',(-0.0344330127020152,-0.0169885018748211,-0.00158629940353296));
#15435=CARTESIAN_POINT('',(-0.0344330127020152,-0.0169885018585916,0.00158629957734368));
#15436=CARTESIAN_POINT('',(-0.034433012702032,-0.0161625394129158,0.00453196473047549));
#15437=CARTESIAN_POINT('',(-0.0344330130224785,-0.0161625399943182,-0.00453196471513884));
#15438=CARTESIAN_POINT('',(-0.0342520086861361,-0.015881055117015,-0.00460738836069848));
#15439=CARTESIAN_POINT('',(-0.0343218322129477,-0.0159691905510249,-0.00458377254232949));
#15440=CARTESIAN_POINT('',(-0.0343819208988127,-0.016063166488791,-0.00455859176569555));
#15441=CARTESIAN_POINT('',(-0.0344330130226463,-0.0161625399939248,-0.00453196471524426));
#15442=CARTESIAN_POINT('',(-0.0342520087102228,-0.0158810549904241,-0.00460738839225635));
#15443=CARTESIAN_POINT('',(-0.0342520085854105,-0.0119306428896003,-0.0114497028629186));
#15444=CARTESIAN_POINT('',(-0.0342520085854116,-0.0137719995107036,-0.00953100081964178));
#15445=CARTESIAN_POINT('',(-0.0342520085854223,-0.0151400885896553,-0.00716140102534911));
#15446=CARTESIAN_POINT('',(-0.0342520085854456,-0.0158810549906252,-0.00460738839231471));
#15447=CARTESIAN_POINT('',(-0.034252008901483,-0.0119306429110209,-0.0114497029404512));
#15448=CARTESIAN_POINT('',(-0.0344330130226575,-0.0120060665709592,-0.0117311878677442));
#15449=CARTESIAN_POINT('',(-0.0343819209629934,-0.0119794395538897,-0.0116318144871932));
#15450=CARTESIAN_POINT('',(-0.0343218321466391,-0.0119542587212024,-0.0115378383439048));
#15451=CARTESIAN_POINT('',(-0.0342520087094023,-0.0119306429320419,-0.0114497030189024));
#15452=CARTESIAN_POINT('',(-0.0344330128623293,-0.0120060664878185,-0.0117311875537928));
#15453=CARTESIAN_POINT('',(-0.0344330127020451,-0.00415647328947946,-0.0162631520429359));
#15454=CARTESIAN_POINT('',(-0.034433012702027,-0.00712047535574833,-0.0155056238968224));
#15455=CARTESIAN_POINT('',(-0.0344330127020133,-0.00986802665890055,-0.0139193243939388));
#15456=CARTESIAN_POINT('',(-0.0344330127020119,-0.0120060662886953,-0.0117311873592286));
#15457=CARTESIAN_POINT('',(-0.0442000000003118,0.01,-0.017320508075658));
#15458=CARTESIAN_POINT('',(-0.0442000000003118,0.01,-0.017320508075658));
#15459=CARTESIAN_POINT('',(-0.044199999875144,0.00813804538124414,-0.0183955080746721));
#15460=CARTESIAN_POINT('',(-0.0442000000002041,0.01,-0.015170508075624));
#15461=CARTESIAN_POINT('',(-0.0442000000001921,0.01,-0.015170508075624));
#15462=CARTESIAN_POINT('',(-0.044200000000204,0.00924950842193217,-0.015170508075624));
#15463=CARTESIAN_POINT('',(-0.0442000000002087,0.00776993675738555,-0.0160329804609734));
#15464=CARTESIAN_POINT('',(-0.0442000000001946,0.00776279959244236,-0.0177455633018591));
#15465=CARTESIAN_POINT('',(-0.0442000000001921,0.00813804538092926,-0.0183955080741079));
#15466=CARTESIAN_POINT('',(-0.0442000000001119,0.0200000000003509,9.42587836741818E-20));
#15467=CARTESIAN_POINT('',(-0.0442000000001119,0.0200000000003509,9.42587836741817E-20));
#15468=CARTESIAN_POINT('',(-0.044199999875096,0.0199999999995591,-0.00214999999980227));
#15469=CARTESIAN_POINT('',(-0.044199999875096,0.02,0.00214999999980227));
#15470=CARTESIAN_POINT('',(-0.0442000000001921,0.02,0.00214999999960454));
#15471=CARTESIAN_POINT('',(-0.0443570796329555,0.0200000000000128,0.00214999999964654));
#15472=CARTESIAN_POINT('',(-0.0445000000003256,0.0200000000000035,0.00229292036704452));
#15473=CARTESIAN_POINT('',(-0.0445000000003369,0.02,0.00244999999980785));
#15474=CARTESIAN_POINT('',(-0.0445000000003369,0.02,-0.00244999999980785));
#15475=CARTESIAN_POINT('',(-0.0445000000003255,0.0200000000000035,-0.00229292036704452));
#15476=CARTESIAN_POINT('',(-0.0443570796329555,0.0200000000000127,-0.00214999999964655));
#15477=CARTESIAN_POINT('',(-0.0442000000001921,0.02,-0.00214999999960454));
#15478=CARTESIAN_POINT('',(-0.0442000000001119,0.0199999999996491,-3.34075843811147E-19));
#15479=CARTESIAN_POINT('',(-0.0442000000001921,0.02,0.00214999999960455));
#15480=CARTESIAN_POINT('',(-0.0442000000002049,0.0194371313163136,0.00214999999969641));
#15481=CARTESIAN_POINT('',(-0.0442000000002303,0.0183158751829514,0.00168476499344337));
#15482=CARTESIAN_POINT('',(-0.0442000000002463,0.0176170624086775,2.44360809131443E-13));
#15483=CARTESIAN_POINT('',(-0.0442000000002303,0.0183158751826059,-0.00168476499309796));
#15484=CARTESIAN_POINT('',(-0.0442000000002049,0.0194371313158727,-0.00214999999958097));
#15485=CARTESIAN_POINT('',(-0.0442000000001921,0.0199999999995591,-0.00214999999960455));
#15486=CARTESIAN_POINT('',(-0.0442000000003118,0.01,0.017320508075658));
#15487=CARTESIAN_POINT('',(-0.0442000000001921,0.01,0.019470508075692));
#15488=CARTESIAN_POINT('',(-0.0442000000001842,0.00924950842153377,0.019470508075692));
#15489=CARTESIAN_POINT('',(-0.0442000000001857,0.00851329117083413,0.0190454528477522));
#15490=CARTESIAN_POINT('',(-0.0442000000001921,0.00813804538168881,0.0183955080754235));
#15491=CARTESIAN_POINT('',(-0.0442000000001565,0.01,0.019470508075692));
#15492=CARTESIAN_POINT('',(-0.044199999875,0.00813804538167257,0.0183955080754328));
#15493=CARTESIAN_POINT('',(-0.0442,0.01,0.017320508076));
#15494=CARTESIAN_POINT('',(-0.044199999875096,0.0118619546182749,0.016245508076153));
#15495=CARTESIAN_POINT('',(-0.0442000000001684,0.01,0.017320508075658));
#15496=CARTESIAN_POINT('',(-0.0442000000003118,-0.01,0.017320508075658));
#15497=CARTESIAN_POINT('',(-0.0442000000001921,-0.00999999999999999,0.019470508075692));
#15498=CARTESIAN_POINT('',(-0.0442000000001802,-0.0107504915780945,0.019470508075692));
#15499=CARTESIAN_POINT('',(-0.0442000000001755,-0.0122300632426902,0.0186080356902759));
#15500=CARTESIAN_POINT('',(-0.0442000000001896,-0.0122372004075394,0.0168954528493138));
#15501=CARTESIAN_POINT('',(-0.0442000000001921,-0.0118619546189909,0.0162455080770697));
#15502=CARTESIAN_POINT('',(-0.0442000000001803,-0.01,0.019470508075692));
#15503=CARTESIAN_POINT('',(-0.044199999875,-0.0118619546176726,0.0162455080754329));
#15504=CARTESIAN_POINT('',(-0.0442,-0.01,0.017320508076));
#15505=CARTESIAN_POINT('',(-0.044199999875096,-0.00813804538124414,0.0183955080746721));
#15506=CARTESIAN_POINT('',(-0.044200000000216,-0.01,0.017320508075658));
#15507=CARTESIAN_POINT('',(-0.0442000000001119,-0.0199999999996491,3.6189501084092E-19));
#15508=CARTESIAN_POINT('',(-0.0442000000001119,-0.0199999999996491,3.6189501084092E-19));
#15509=CARTESIAN_POINT('',(-0.044199999875096,-0.0199999999998069,-0.00214999999980227));
#15510=CARTESIAN_POINT('',(-0.044199999875096,-0.0199999999995591,0.00214999999980227));
#15511=CARTESIAN_POINT('',(-0.0442000000001921,-0.02,0.00214999999960455));
#15512=CARTESIAN_POINT('',(-0.0443570796329555,-0.0199999999999872,0.00214999999964654));
#15513=CARTESIAN_POINT('',(-0.0445000000003255,-0.0199999999999965,0.00229292036704452));
#15514=CARTESIAN_POINT('',(-0.0445000000003369,-0.02,0.00244999999980786));
#15515=CARTESIAN_POINT('',(-0.0445000000003369,-0.02,-0.00244999999980786));
#15516=CARTESIAN_POINT('',(-0.0445000000003255,-0.0199999999999965,-0.00229292036704452));
#15517=CARTESIAN_POINT('',(-0.0443570796329555,-0.0199999999999872,-0.00214999999964655));
#15518=CARTESIAN_POINT('',(-0.0442000000001921,-0.02,-0.00214999999960455));
#15519=CARTESIAN_POINT('',(-0.0442000000001119,-0.0200000000003509,-1.67275847704353E-19));
#15520=CARTESIAN_POINT('',(-0.0442000000001922,-0.0200000000003509,-1.6727584759041E-19));
#15521=CARTESIAN_POINT('',(-0.0442000000003118,-0.01,-0.017320508075658));
#15522=CARTESIAN_POINT('',(-0.0442000000001921,-0.00813804538092926,-0.0183955080741079));
#15523=CARTESIAN_POINT('',(-0.0442000000001946,-0.00776279959244236,-0.017745563301859));
#15524=CARTESIAN_POINT('',(-0.0442000000002087,-0.00776993675738556,-0.0160329804609734));
#15525=CARTESIAN_POINT('',(-0.044200000000204,-0.00924950842193217,-0.015170508075624));
#15526=CARTESIAN_POINT('',(-0.0442000000001921,-0.01,-0.015170508075624));
#15527=CARTESIAN_POINT('',(-0.044199999875096,-0.00813804538146463,-0.018395508075054));
#15528=CARTESIAN_POINT('',(-0.0442000000002758,-0.01,-0.015170508075624));
#15529=CARTESIAN_POINT('',(-0.0442000000003118,-0.01,-0.017320508075658));
#15530=CARTESIAN_POINT('',(-0.0393760042937274,-0.012974499756,0.0153454297215));
#15531=CARTESIAN_POINT('',(-0.0384862022102034,-0.0140183571386411,0.0192411585091307));
#15532=CARTESIAN_POINT('',(-0.0370999087763453,-0.013352347141783,0.0167555753626619));
#15533=CARTESIAN_POINT('',(-0.035733240200822,-0.0126836892229704,0.0142601100369248));
#15534=CARTESIAN_POINT('',(-0.0344330130228521,-0.0120060665701493,0.0117311878683936));
#15535=CARTESIAN_POINT('',(-0.0384862022685832,-0.0140183571306401,0.0192411584797665));
#15536=CARTESIAN_POINT('',(-0.0444805635282456,-0.014018356622,0.019241156581));
#15537=CARTESIAN_POINT('',(-0.0424824431083581,-0.014018356622,0.019241156581));
#15538=CARTESIAN_POINT('',(-0.0404843226884707,-0.014018356622,0.019241156581));
#15539=CARTESIAN_POINT('',(-0.0384862022685832,-0.014018356622,0.019241156581));
#15540=CARTESIAN_POINT('',(-0.0444805635319336,-0.0140183566169593,0.019241156562634));
#15541=CARTESIAN_POINT('',(-0.0445000000129707,-0.0139888823224751,0.0191311570460743));
#15542=CARTESIAN_POINT('',(-0.0445000000166381,-0.0139989932774539,0.0191688916437659));
#15543=CARTESIAN_POINT('',(-0.0444935802519982,-0.0140088206617122,0.0192055678927093));
#15544=CARTESIAN_POINT('',(-0.044480563533571,-0.0140183566158597,0.0192411565580842));
#15545=CARTESIAN_POINT('',(-0.034252008839487,-0.01193064289,0.011449702862));
#15546=CARTESIAN_POINT('',(-0.0376680058929914,-0.01193064289,0.011449702862));
#15547=CARTESIAN_POINT('',(-0.0410840029464957,-0.01193064289,0.011449702862));
#15548=CARTESIAN_POINT('',(-0.0445,-0.01193064289,0.011449702862));
#15549=CARTESIAN_POINT('',(-0.0442000000055845,-1.31051679305457E-11,2.57086317240235E-11));
#15550=CARTESIAN_POINT('',(-0.0444805635188123,-0.0140183566003539,0.0192411565622842));
#15551=CARTESIAN_POINT('',(-0.0444283437647183,-0.0140566124263418,0.0193839292026706));
#15552=CARTESIAN_POINT('',(-0.0443084984770918,-0.0139913606486926,0.0195000961256288));
#15553=CARTESIAN_POINT('',(-0.0442000000005702,-0.0139023583532664,0.0195633440958977));
#15554=CARTESIAN_POINT('',(-0.0441999998126405,-0.0139023583539755,0.0195633440953938));
#15555=CARTESIAN_POINT('',(-0.0442000000001921,-0.0139023583537827,0.0195633440951225));
#15556=CARTESIAN_POINT('',(-0.0442000000001617,-0.0126734170487115,0.0204366703701264));
#15557=CARTESIAN_POINT('',(-0.0442000000001615,-0.0113619671847084,0.0211938363022351));
#15558=CARTESIAN_POINT('',(-0.0442000000001921,-0.00999117379229732,0.0218214675548383));
#15559=CARTESIAN_POINT('',(-0.0441999998752201,-0.00999117379233075,0.0218214675549114));
#15560=CARTESIAN_POINT('',(-0.0442000000004402,-0.00999117379338535,0.0218214675543966));
#15561=CARTESIAN_POINT('',(-0.0443082283281583,-0.00989214828484741,0.0218668073585679));
#15562=CARTESIAN_POINT('',(-0.0444284338973912,-0.00975848851517938,0.0218651676816527));
#15563=CARTESIAN_POINT('',(-0.044480563529604,-0.00965415207773743,0.0217608312354494));
#15564=CARTESIAN_POINT('',(-0.0444805634409269,-0.00965415208178998,0.02176083123879));
#15565=CARTESIAN_POINT('',(-0.0444805635173688,-0.00965415208444921,0.0217608312191856));
#15566=CARTESIAN_POINT('',(-0.044493580238476,-0.00962809936884818,0.0217347785035891));
#15567=CARTESIAN_POINT('',(-0.0445000000034239,-0.00960125048409792,0.0217079296411072));
#15568=CARTESIAN_POINT('',(-0.0445000000002923,-0.00957362683652262,0.0216803059935367));
#15569=CARTESIAN_POINT('',(-0.0393760042937274,-0.00680228209300001,0.0189089612505));
#15570=CARTESIAN_POINT('',(-0.0384862032523497,-0.009654152087,0.021760831244));
#15571=CARTESIAN_POINT('',(-0.040484323344315,-0.009654152087,0.021760831244));
#15572=CARTESIAN_POINT('',(-0.0424824434362803,-0.009654152087,0.021760831244));
#15573=CARTESIAN_POINT('',(-0.0444805635282456,-0.009654152087,0.021760831244));
#15574=CARTESIAN_POINT('',(-0.0384862032523497,-0.00965415458831338,0.0217608337456173));
#15575=CARTESIAN_POINT('',(-0.0344330130247402,-0.00415647342820006,0.016263152586164));
#15576=CARTESIAN_POINT('',(-0.0357332404762259,-0.00600777333354867,0.018114452491188));
#15577=CARTESIAN_POINT('',(-0.0370999095145224,-0.00783458133811811,0.0199412604954371));
#15578=CARTESIAN_POINT('',(-0.0384862032521895,-0.00965415486626073,0.0217608340232608));
#15579=CARTESIAN_POINT('',(-0.044499999875,-0.00395041209900001,0.016057091257));
#15580=CARTESIAN_POINT('',(-0.0410840028840801,-0.00395041209900001,0.016057091257));
#15581=CARTESIAN_POINT('',(-0.0376680058931603,-0.00395041209900001,0.016057091257));
#15582=CARTESIAN_POINT('',(-0.0342520089022404,-0.00395041209900001,0.016057091257));
#15583=CARTESIAN_POINT('',(-0.0295,0.,0.));
#15584=CARTESIAN_POINT('',(-0.04449999975,0.00395041209500243,0.0160570912583414));
#15585=CARTESIAN_POINT('',(-0.0410840027783333,0.00395041209500243,0.0160570912583414));
#15586=CARTESIAN_POINT('',(-0.0376680058066667,0.00395041209500243,0.0160570912583414));
#15587=CARTESIAN_POINT('',(-0.034252008835,0.00395041209500243,0.0160570912583414));
#15588=CARTESIAN_POINT('',(-0.0393760042937274,0.00680228209300001,0.0189089612505));
#15589=CARTESIAN_POINT('',(-0.0384862022100965,0.00965415349846632,0.0217608326554663));
#15590=CARTESIAN_POINT('',(-0.0370999087769037,0.0078345803494711,0.0199412595067901));
#15591=CARTESIAN_POINT('',(-0.0357332402020445,0.00600777294316644,0.0181144521008057));
#15592=CARTESIAN_POINT('',(-0.0344330130246683,0.00415647342809768,0.0162631525860615));
#15593=CARTESIAN_POINT('',(-0.0384862022685706,0.00965415347674228,0.02176083263408));
#15594=CARTESIAN_POINT('',(-0.0444805635282456,0.009654152087,0.021760831244));
#15595=CARTESIAN_POINT('',(-0.0424824431083539,0.009654152087,0.021760831244));
#15596=CARTESIAN_POINT('',(-0.0404843226884622,0.009654152087,0.021760831244));
#15597=CARTESIAN_POINT('',(-0.0384862022685706,0.009654152087,0.021760831244));
#15598=CARTESIAN_POINT('',(-0.0444805635304399,0.00965415207631084,0.0217608312336668));
#15599=CARTESIAN_POINT('',(-0.0445000000193966,0.00957362685480404,0.0216803059848004));
#15600=CARTESIAN_POINT('',(-0.0445000000226021,0.0096012504979128,0.0217079296279044));
#15601=CARTESIAN_POINT('',(-0.0444935802508817,0.00962809936227532,0.0217347785192799));
#15602=CARTESIAN_POINT('',(-0.0444805635321006,0.0096541520732335,0.0217608312302335));
#15603=CARTESIAN_POINT('',(-0.0442000000055845,1.31053917940051E-11,2.57091155293273E-11));
#15604=CARTESIAN_POINT('',(-0.0444805635171393,0.00965415208412121,0.021760831219211));
#15605=CARTESIAN_POINT('',(-0.0444283878394043,0.00975858068479965,0.0218652598335098));
#15606=CARTESIAN_POINT('',(-0.0443084084393283,0.00989198348882134,0.0218668828120512));
#15607=CARTESIAN_POINT('',(-0.0442000000004402,0.00999117379338535,0.0218214675543966));
#15608=CARTESIAN_POINT('',(-0.044199999844711,0.00999117381829546,0.0218214675430476));
#15609=CARTESIAN_POINT('',(-0.0442000000001922,0.00999117381825278,0.0218214675429544));
#15610=CARTESIAN_POINT('',(-0.0442000000001615,0.0113619671891927,0.0211938362982097));
#15611=CARTESIAN_POINT('',(-0.0442000000001618,0.0126734170333715,0.0204366703779577));
#15612=CARTESIAN_POINT('',(-0.0442000000001922,0.0139023583213122,0.0195633441181971));
#15613=CARTESIAN_POINT('',(-0.0441999997741247,0.013902358321505,0.0195633441184683));
#15614=CARTESIAN_POINT('',(-0.0444805635187775,0.014018356600366,0.0192411565623608));
#15615=CARTESIAN_POINT('',(-0.0444283437696937,0.0140566124226209,0.0193839291889622));
#15616=CARTESIAN_POINT('',(-0.0443084984666164,0.0139913606401035,0.0195000961317325));
#15617=CARTESIAN_POINT('',(-0.0442000000005702,0.0139023583532664,0.0195633440958977));
#15618=CARTESIAN_POINT('',(-0.0444805634416584,0.0140183566195451,0.0192411565718381));
#15619=CARTESIAN_POINT('',(-0.0444805635186538,0.0140183566004662,0.0192411565622887));
#15620=CARTESIAN_POINT('',(-0.0444935802393538,0.0140088206446543,0.0192055678907021));
#15621=CARTESIAN_POINT('',(-0.0445000000040598,0.0139989932902217,0.0191688916430041));
#15622=CARTESIAN_POINT('',(-0.0445000000004408,0.0139888823334323,0.0191311570385554));
#15623=CARTESIAN_POINT('',(-0.0393760042937274,0.012974499756,0.0153454297215));
#15624=CARTESIAN_POINT('',(-0.0384862032524104,0.014018356622,0.019241156581));
#15625=CARTESIAN_POINT('',(-0.0404843233443555,0.014018356622,0.019241156581));
#15626=CARTESIAN_POINT('',(-0.0424824434363005,0.014018356622,0.019241156581));
#15627=CARTESIAN_POINT('',(-0.0444805635282456,0.014018356622,0.019241156581));
#15628=CARTESIAN_POINT('',(-0.0384862032524104,0.014018357537509,0.0192411599981722));
#15629=CARTESIAN_POINT('',(-0.0344330130229279,0.0120060665701866,0.0117311878685389));
#15630=CARTESIAN_POINT('',(-0.0357332404750095,0.0126836893658611,0.0142601105702061));
#15631=CARTESIAN_POINT('',(-0.0370999095139687,0.0133523475036553,0.0167555767131877));
#15632=CARTESIAN_POINT('',(-0.0384862032523048,0.0140183576392926,0.0192411603775878));
#15633=CARTESIAN_POINT('',(-0.0445,0.01193064289,0.011449702862));
#15634=CARTESIAN_POINT('',(-0.041084002967161,0.01193064289,0.011449702862));
#15635=CARTESIAN_POINT('',(-0.037668005934322,0.01193064289,0.011449702862));
#15636=CARTESIAN_POINT('',(-0.034252008901483,0.01193064289,0.011449702862));
#15637=CARTESIAN_POINT('',(-0.0295,0.,0.));
#15638=CARTESIAN_POINT('',(-0.044199999749838,0.0158810549872041,0.00460738840260347));
#15639=CARTESIAN_POINT('',(-0.0408840027782253,0.0158810549872041,0.00460738840260347));
#15640=CARTESIAN_POINT('',(-0.0375680058066127,0.0158810549872041,0.00460738840260347));
#15641=CARTESIAN_POINT('',(-0.034252008835,0.0158810549872041,0.00460738840260347));
#15642=CARTESIAN_POINT('',(-0.0441999999375076,0.0158810551716672,0.00460738834575336));
#15643=CARTESIAN_POINT('',(-0.0441999998749613,0.0158810549895393,0.00460738839455436));
#15644=CARTESIAN_POINT('',(-0.0443716844373847,0.0158810549662353,0.00460738847488032));
#15645=CARTESIAN_POINT('',(-0.044500000000068,0.0159304182122806,0.00443700078956962));
#15646=CARTESIAN_POINT('',(-0.0444999999992906,0.0159746109794523,0.00427173728759232));
#15647=CARTESIAN_POINT('',(-0.0442,0.024530335195,0.001979237895));
#15648=CARTESIAN_POINT('',(-0.0442000000000539,0.0236725084664752,0.00251967472754294));
#15649=CARTESIAN_POINT('',(-0.0442000000000539,0.0210753573886682,0.00321557926146354));
#15650=CARTESIAN_POINT('',(-0.0442000000000539,0.0184782063108613,0.00391148379538414));
#15651=CARTESIAN_POINT('',(-0.0442000000000539,0.0158810552330543,0.00460738832930474));
#15652=CARTESIAN_POINT('',(-0.0441999999985952,0.0236725087085416,0.00251967466285297));
#15653=CARTESIAN_POINT('',(-0.0442,0.0235948629946094,0.00222989691563664));
#15654=CARTESIAN_POINT('',(-0.0442000000067454,4.40013553093732E-11,8.52580180210794E-13));
#15655=CARTESIAN_POINT('',(-0.0442000000002482,0.0235948629947446,0.00222989691525306));
#15656=CARTESIAN_POINT('',(-0.044199999875096,0.0238935321461809,0.00225812346418508));
#15657=CARTESIAN_POINT('',(-0.0442000000067717,4.40013553093804E-11,8.52580180210556E-13));
#15658=CARTESIAN_POINT('',(-0.0441999997689131,0.0238935321508499,-0.00225812341441558));
#15659=CARTESIAN_POINT('',(-0.0444805635187719,0.0236725086811496,-0.00251967465380841));
#15660=CARTESIAN_POINT('',(-0.0444283437697893,0.0238152813140498,-0.00248141885441365));
#15661=CARTESIAN_POINT('',(-0.0443084995967842,0.0238832590521061,-0.00236682456350268));
#15662=CARTESIAN_POINT('',(-0.0442000000002077,0.0238935321467111,-0.00225812345827953));
#15663=CARTESIAN_POINT('',(-0.044480563441677,0.023672508698868,-0.00251967466544691));
#15664=CARTESIAN_POINT('',(-0.0444805635187868,0.0236725086811511,-0.00251967465379354));
#15665=CARTESIAN_POINT('',(-0.0444935802398986,0.0236369200083081,-0.0025292106099421));
#15666=CARTESIAN_POINT('',(-0.0445000000044559,0.023600243767542,-0.00253903799543801));
#15667=CARTESIAN_POINT('',(-0.0445000000003558,0.023562509161789,-0.00254914895257684));
#15668=CARTESIAN_POINT('',(-0.0393760042937274,0.0197767818485,-0.003563531529));
#15669=CARTESIAN_POINT('',(-0.044499999875,0.015881054989,-0.004607388395));
#15670=CARTESIAN_POINT('',(-0.0410840028839326,0.015881054989,-0.004607388395));
#15671=CARTESIAN_POINT('',(-0.0376680058928653,0.015881054989,-0.004607388395));
#15672=CARTESIAN_POINT('',(-0.0342520089017979,0.015881054989,-0.004607388395));
#15673=CARTESIAN_POINT('',(-0.0384862032524471,0.023672508708,-0.002519674663));
#15674=CARTESIAN_POINT('',(-0.0404843233443799,0.023672508708,-0.002519674663));
#15675=CARTESIAN_POINT('',(-0.0424824434363127,0.023672508708,-0.002519674663));
#15676=CARTESIAN_POINT('',(-0.0444805635282456,0.023672508708,-0.002519674663));
#15677=CARTESIAN_POINT('',(-0.038486203252447,0.0236725121255199,-0.00251967374727935));
#15678=CARTESIAN_POINT('',(-0.0344330129932801,0.0161625399382474,-0.00453196473016298));
#15679=CARTESIAN_POINT('',(-0.0357332404541263,0.0186914626596971,-0.00385434192918779));
#15680=CARTESIAN_POINT('',(-0.0370999095034317,0.0211869288216903,-0.00318568378630103));
#15681=CARTESIAN_POINT('',(-0.0384862032523079,0.0236725125049948,-0.0025196736455983));
#15682=CARTESIAN_POINT('',(-0.0295,0.,0.));
#15683=CARTESIAN_POINT('',(-0.04449999975,0.0119306428861598,-0.0114497028660997));
#15684=CARTESIAN_POINT('',(-0.0410840027783333,0.0119306428861598,-0.0114497028660997));
#15685=CARTESIAN_POINT('',(-0.0376680058066667,0.0119306428861598,-0.0114497028660997));
#15686=CARTESIAN_POINT('',(-0.034252008835,0.0119306428861598,-0.0114497028660997));
#15687=CARTESIAN_POINT('',(-0.0393760042937274,0.012974499756,-0.0153454297215));
#15688=CARTESIAN_POINT('',(-0.0384862022102251,0.0140183571386519,-0.0192411585091713));
#15689=CARTESIAN_POINT('',(-0.037099908776487,0.0133523471418517,-0.0167555753629181));
#15690=CARTESIAN_POINT('',(-0.035733240201101,0.0126836892231061,-0.0142601100374313));
#15691=CARTESIAN_POINT('',(-0.0344330130232636,0.0120060665703642,-0.0117311878691955));
#15692=CARTESIAN_POINT('',(-0.0384862022686053,0.0140183571306509,-0.0192411584798069));
#15693=CARTESIAN_POINT('',(-0.0444805635282456,0.014018356622,-0.019241156581));
#15694=CARTESIAN_POINT('',(-0.0424824431083655,0.014018356622,-0.019241156581));
#15695=CARTESIAN_POINT('',(-0.0404843226884854,0.014018356622,-0.019241156581));
#15696=CARTESIAN_POINT('',(-0.0384862022686053,0.014018356622,-0.019241156581));
#15697=CARTESIAN_POINT('',(-0.0444805635319414,0.0140183566169537,-0.0192411565626129));
#15698=CARTESIAN_POINT('',(-0.0445000000129707,0.0139888823224751,-0.0191311570460743));
#15699=CARTESIAN_POINT('',(-0.044500000016638,0.0139989932774517,-0.0191688916437578));
#15700=CARTESIAN_POINT('',(-0.0444935802520009,0.0140088206617081,-0.0192055678926938));
#15701=CARTESIAN_POINT('',(-0.0444805635335792,0.0140183566158538,-0.0192411565580619));
#15702=CARTESIAN_POINT('',(-0.0442000000055849,1.31055792648314E-11,-2.57092921253891E-11));
#15703=CARTESIAN_POINT('',(-0.0444805635188167,0.014018356600344,-0.019241156562263));
#15704=CARTESIAN_POINT('',(-0.0444283437647304,0.014056612426345,-0.0193839292026541));
#15705=CARTESIAN_POINT('',(-0.0443084984770938,0.0139913606486981,-0.0195000961256248));
#15706=CARTESIAN_POINT('',(-0.0442000000005702,0.0139023583532664,-0.0195633440958977));
#15707=CARTESIAN_POINT('',(-0.0441999998126405,0.0139023583539033,-0.019563344095445));
#15708=CARTESIAN_POINT('',(-0.0442000000001921,0.0139023583537106,-0.0195633440951738));
#15709=CARTESIAN_POINT('',(-0.0442000000001617,0.0126734170595584,-0.0204366703624114));
#15710=CARTESIAN_POINT('',(-0.0442000000001615,0.0113619672079449,-0.0211938362888249));
#15711=CARTESIAN_POINT('',(-0.0442000000001921,0.00999117382876566,-0.021821467538141));
#15712=CARTESIAN_POINT('',(-0.044199999774127,0.00999117382878557,-0.0218214675381844));
#15713=CARTESIAN_POINT('',(-0.0444805635186256,0.00965415208114367,-0.0217608312162303));
#15714=CARTESIAN_POINT('',(-0.0444283437697871,0.00975866889166734,-0.0218653480433214));
#15715=CARTESIAN_POINT('',(-0.044308500011943,0.00989189970270077,-0.0218669211743478));
#15716=CARTESIAN_POINT('',(-0.0442000000004402,0.00999117379338393,-0.0218214675543935));
#15717=CARTESIAN_POINT('',(-0.0444805634416919,0.00965415208025887,-0.0217608312372589));
#15718=CARTESIAN_POINT('',(-0.0444805635188954,0.00965415208138903,-0.0217608312161197));
#15719=CARTESIAN_POINT('',(-0.0444935802389732,0.00962809936671424,-0.0217347785014494));
#15720=CARTESIAN_POINT('',(-0.0445000000034239,0.00960125048298382,-0.0217079296399931));
#15721=CARTESIAN_POINT('',(-0.0445000000002923,0.00957362683652262,-0.0216803059935368));
#15722=CARTESIAN_POINT('',(-0.0393760042937274,0.00680228209300001,-0.0189089612505));
#15723=CARTESIAN_POINT('',(-0.0384862032527067,0.009654152087,-0.021760831244));
#15724=CARTESIAN_POINT('',(-0.040484323344553,0.009654152087,-0.021760831244));
#15725=CARTESIAN_POINT('',(-0.0424824434363993,0.009654152087,-0.021760831244));
#15726=CARTESIAN_POINT('',(-0.0444805635282456,0.009654152087,-0.021760831244));
#15727=CARTESIAN_POINT('',(-0.0384862032527067,0.00965415458873634,-0.0217608337460403));
#15728=CARTESIAN_POINT('',(-0.0344330130250192,0.00415647342859888,-0.0162631525865627));
#15729=CARTESIAN_POINT('',(-0.0357332404765253,0.00600777333395774,-0.018114452491597));
#15730=CARTESIAN_POINT('',(-0.0370999095149851,0.00783458133873632,-0.0199412604960553));
#15731=CARTESIAN_POINT('',(-0.0384862032526683,0.00965415486689057,-0.0217608340238905));
#15732=CARTESIAN_POINT('',(-0.044499999875,0.00395041209900001,-0.016057091257));
#15733=CARTESIAN_POINT('',(-0.0410840028840801,0.00395041209900001,-0.016057091257));
#15734=CARTESIAN_POINT('',(-0.0376680058931603,0.00395041209900001,-0.016057091257));
#15735=CARTESIAN_POINT('',(-0.0342520089022404,0.00395041209900001,-0.016057091257));
#15736=CARTESIAN_POINT('',(-0.0295,0.,0.));
#15737=CARTESIAN_POINT('',(-0.04449999975,-0.00395041210158917,-0.0160570912567209));
#15738=CARTESIAN_POINT('',(-0.0410840027783333,-0.00395041210158917,-0.0160570912567209));
#15739=CARTESIAN_POINT('',(-0.0376680058066667,-0.00395041210158917,-0.0160570912567209));
#15740=CARTESIAN_POINT('',(-0.034252008835,-0.00395041210158917,-0.0160570912567209));
#15741=CARTESIAN_POINT('',(-0.0393760042937274,-0.00680228209300001,-0.0189089612505));
#15742=CARTESIAN_POINT('',(-0.0384862022103422,-0.00965415349879022,-0.0217608326557902));
#15743=CARTESIAN_POINT('',(-0.037099908777168,-0.00783458034982418,-0.0199412595071432));
#15744=CARTESIAN_POINT('',(-0.0357332402023234,-0.00600777294354627,-0.0181144521011855));
#15745=CARTESIAN_POINT('',(-0.0344330130249473,-0.0041564734284965,-0.0162631525864603));
#15746=CARTESIAN_POINT('',(-0.0384862022688168,-0.00965415347706603,-0.0217608326344038));
#15747=CARTESIAN_POINT('',(-0.0444805635282456,-0.009654152087,-0.021760831244));
#15748=CARTESIAN_POINT('',(-0.042482443108436,-0.009654152087,-0.021760831244));
#15749=CARTESIAN_POINT('',(-0.0404843226886264,-0.009654152087,-0.021760831244));
#15750=CARTESIAN_POINT('',(-0.0384862022688168,-0.009654152087,-0.021760831244));
#15751=CARTESIAN_POINT('',(-0.044480563531975,-0.00965415207323825,-0.0217608312305942));
#15752=CARTESIAN_POINT('',(-0.0445000000193967,-0.00957362685480405,-0.0216803059848005));
#15753=CARTESIAN_POINT('',(-0.044500000022602,-0.00960125049679463,-0.0217079296267862));
#15754=CARTESIAN_POINT('',(-0.0444935802513844,-0.00962809936013126,-0.0217347785171359));
#15755=CARTESIAN_POINT('',(-0.0444805635336362,-0.00965415207016007,-0.0217608312271601));
#15756=CARTESIAN_POINT('',(-0.0442000000055833,-1.31055491163998E-11,-2.57092734960733E-11));
#15757=CARTESIAN_POINT('',(-0.0444805635186711,-0.00965415208105065,-0.0217608312161348));
#15758=CARTESIAN_POINT('',(-0.0444283437648285,-0.00975866890166532,-0.0218653480534098));
#15759=CARTESIAN_POINT('',(-0.0443085000224662,-0.00989189969309658,-0.0218669211787452));
#15760=CARTESIAN_POINT('',(-0.0442000000004402,-0.00999117379338393,-0.0218214675543935));
#15761=CARTESIAN_POINT('',(-0.0441999998126405,-0.00999117379246263,-0.0218214675548153));
#15762=CARTESIAN_POINT('',(-0.0442000000001921,-0.00999117379244271,-0.0218214675547718));
#15763=CARTESIAN_POINT('',(-0.0442000000001615,-0.0113619671727517,-0.0211938363076986));
#15764=CARTESIAN_POINT('',(-0.0442000000001617,-0.0126734170257031,-0.0204366703834131));
#15765=CARTESIAN_POINT('',(-0.0442000000001921,-0.013902358321375,-0.0195633441181525));
#15766=CARTESIAN_POINT('',(-0.0441999997741401,-0.0139023583215678,-0.0195633441184237));
#15767=CARTESIAN_POINT('',(-0.0444805635187713,-0.0140183566003803,-0.0192411565623913));
#15768=CARTESIAN_POINT('',(-0.0444283437696747,-0.0140566124226176,-0.0193839291889904));
#15769=CARTESIAN_POINT('',(-0.0443084984666218,-0.0139913606400945,-0.0195000961317389));
#15770=CARTESIAN_POINT('',(-0.0442000000005701,-0.0139023583532664,-0.0195633440958977));
#15771=CARTESIAN_POINT('',(-0.0444805634416528,-0.0140183566195491,-0.0192411565718533));
#15772=CARTESIAN_POINT('',(-0.0444805635186475,-0.0140183566004804,-0.0192411565623192));
#15773=CARTESIAN_POINT('',(-0.0444935802393554,-0.0140088206446659,-0.0192055678907229));
#15774=CARTESIAN_POINT('',(-0.0445000000040597,-0.0139989932902247,-0.0191688916430152));
#15775=CARTESIAN_POINT('',(-0.0445000000004407,-0.0139888823334323,-0.0191311570385554));
#15776=CARTESIAN_POINT('',(-0.0393760042937274,-0.012974499756,-0.0153454297215));
#15777=CARTESIAN_POINT('',(-0.0384862032529767,-0.014018356622,-0.019241156581));
#15778=CARTESIAN_POINT('',(-0.040484323344733,-0.014018356622,-0.019241156581));
#15779=CARTESIAN_POINT('',(-0.0424824434364893,-0.014018356622,-0.019241156581));
#15780=CARTESIAN_POINT('',(-0.0444805635282456,-0.014018356622,-0.019241156581));
#15781=CARTESIAN_POINT('',(-0.0384862032529767,-0.0140183575377542,-0.0192411599990874));
#15782=CARTESIAN_POINT('',(-0.0344330130222391,-0.0120060665706653,-0.011731187868038));
#15783=CARTESIAN_POINT('',(-0.0357332404745547,-0.0126836893664783,-0.0142601105702223));
#15784=CARTESIAN_POINT('',(-0.0370999095143791,-0.0133523475038579,-0.0167555767139436));
#15785=CARTESIAN_POINT('',(-0.0384862032529973,-0.0140183576396257,-0.019241160378831));
#15786=CARTESIAN_POINT('',(-0.044499999875,-0.01193064289,-0.011449702862));
#15787=CARTESIAN_POINT('',(-0.0410840028838277,-0.01193064289,-0.011449702862));
#15788=CARTESIAN_POINT('',(-0.0376680058926553,-0.01193064289,-0.011449702862));
#15789=CARTESIAN_POINT('',(-0.034252008901483,-0.01193064289,-0.011449702862));
#15790=CARTESIAN_POINT('',(-0.0295,0.,0.));
#15791=CARTESIAN_POINT('',(-0.04449999975,-0.0158810549890941,-0.00460738839608896));
#15792=CARTESIAN_POINT('',(-0.0410840027783333,-0.0158810549890941,-0.00460738839608896));
#15793=CARTESIAN_POINT('',(-0.0376680058066667,-0.0158810549890941,-0.00460738839608896));
#15794=CARTESIAN_POINT('',(-0.034252008835,-0.0158810549890941,-0.00460738839608896));
#15795=CARTESIAN_POINT('',(-0.0393760042937274,-0.0197767818485,-0.003563531529));
#15796=CARTESIAN_POINT('',(-0.0384862022101706,-0.0236725106364736,-0.00251967414626707));
#15797=CARTESIAN_POINT('',(-0.0370999087760845,-0.0211869274895885,-0.00318568414323665));
#15798=CARTESIAN_POINT('',(-0.0357332402003217,-0.0186914621634017,-0.00385434206216974));
#15799=CARTESIAN_POINT('',(-0.0344330130221634,-0.0161625399944248,-0.00453196471511027));
#15800=CARTESIAN_POINT('',(-0.0384862022686588,-0.0236725106070218,-0.00251967415415977));
#15801=CARTESIAN_POINT('',(-0.0444805635282456,-0.023672508708,-0.002519674663));
#15802=CARTESIAN_POINT('',(-0.0424824431083833,-0.023672508708,-0.002519674663));
#15803=CARTESIAN_POINT('',(-0.0404843226885211,-0.023672508708,-0.002519674663));
#15804=CARTESIAN_POINT('',(-0.0384862022686588,-0.023672508708,-0.002519674663));
#15805=CARTESIAN_POINT('',(-0.0444805635320151,-0.0236725086897196,-0.00251967466791268));
#15806=CARTESIAN_POINT('',(-0.0445000000154798,-0.023562509163137,-0.0025491489365736));
#15807=CARTESIAN_POINT('',(-0.0445000000196407,-0.0236002437613621,-0.00253903798145185));
#15808=CARTESIAN_POINT('',(-0.0444935802521013,-0.0236369200196111,-0.00252921062331408));
#15809=CARTESIAN_POINT('',(-0.0444805635336595,-0.0236725086852255,-0.0025196746691024));
#15810=CARTESIAN_POINT('',(-0.0442000000052978,-1.47752458924516E-11,1.30076225163517E-17));
#15811=CARTESIAN_POINT('',(-0.0444805635188413,-0.0236725086811181,-0.00251967465379378));
#15812=CARTESIAN_POINT('',(-0.0444283437649074,-0.0238152813279393,-0.00248141885068248));
#15813=CARTESIAN_POINT('',(-0.0443085007036546,-0.0238832591538571,-0.00236682348911541));
#15814=CARTESIAN_POINT('',(-0.0441999999998855,-0.0238935321469101,-0.00225812345825258));
#15815=CARTESIAN_POINT('',(-0.0441999965249051,-0.0238935321468263,-0.00225812345938652));
#15816=CARTESIAN_POINT('',(-0.0442000000001921,-0.0238935321468806,-0.00225812345939164));
#15817=CARTESIAN_POINT('',(-0.0442000000001596,-0.0240353842328595,-0.000757165945200664));
#15818=CARTESIAN_POINT('',(-0.0442000000001596,-0.024035384234115,0.000757165905346178));
#15819=CARTESIAN_POINT('',(-0.0442000000001921,-0.0238935321506249,0.00225812341977237));
#15820=CARTESIAN_POINT('',(-0.0441999964978638,-0.0238935321505707,0.00225812341976725));
#15821=CARTESIAN_POINT('',(-0.0444805635187896,-0.0236725086812809,0.00251967465375806));
#15822=CARTESIAN_POINT('',(-0.0444283437698302,-0.0238152813142717,0.00248141885426767));
#15823=CARTESIAN_POINT('',(-0.0443085006931829,-0.0238832591548499,0.00236682347861122));
#15824=CARTESIAN_POINT('',(-0.0441999999998855,-0.0238935321469101,0.00225812345825258));
#15825=CARTESIAN_POINT('',(-0.044480563441692,-0.0236725086989376,0.00251967466542826));
#15826=CARTESIAN_POINT('',(-0.0444805635188046,-0.0236725086812824,0.00251967465374319));
#15827=CARTESIAN_POINT('',(-0.0444935802399076,-0.0236369200084268,0.00252921060989514));
#15828=CARTESIAN_POINT('',(-0.0445000000044733,-0.0236002437676551,0.00253903799540771));
#15829=CARTESIAN_POINT('',(-0.0445000000003707,-0.0235625091618915,0.00254914895254941));
#15830=CARTESIAN_POINT('',(-0.0393760042937274,-0.0197767818485,0.003563531529));
#15831=CARTESIAN_POINT('',(-0.0384862032520929,-0.023672508708,0.002519674663));
#15832=CARTESIAN_POINT('',(-0.0404843233441438,-0.023672508708,0.002519674663));
#15833=CARTESIAN_POINT('',(-0.0424824434361947,-0.023672508708,0.002519674663));
#15834=CARTESIAN_POINT('',(-0.0444805635282456,-0.023672508708,0.002519674663));
#15835=CARTESIAN_POINT('',(-0.0384862032520929,-0.0236725121249481,0.00251967374743256));
#15836=CARTESIAN_POINT('',(-0.0344330130206301,-0.0161625399952047,0.00453196471691751));
#15837=CARTESIAN_POINT('',(-0.0357332404728482,-0.0186914626973602,0.00385434192111219));
#15838=CARTESIAN_POINT('',(-0.0370999095134191,-0.0211869288395885,0.00318568378150523));
#15839=CARTESIAN_POINT('',(-0.0384862032519836,-0.0236725125044133,0.00251967364575413));
#15840=CARTESIAN_POINT('',(-0.044499999875,-0.015881054989,0.004607388395));
#15841=CARTESIAN_POINT('',(-0.0410840028839326,-0.015881054989,0.004607388395));
#15842=CARTESIAN_POINT('',(-0.0376680058928653,-0.015881054989,0.004607388395));
#15843=CARTESIAN_POINT('',(-0.0342520089017979,-0.015881054989,0.004607388395));
#15844=CARTESIAN_POINT('',(-0.0295,0.,0.));
#15845=CARTESIAN_POINT('',(-0.0247416697501165,0.,-9.27109177476128E-16));
#15846=CARTESIAN_POINT('',(-0.0384862032527451,0.00965415486652353,-0.021760834024199));
#15847=CARTESIAN_POINT('',(-0.038494882212823,0.00966554660283219,-0.0217722254619481));
#15848=CARTESIAN_POINT('',(-0.0385033092139225,0.00967786860797711,-0.0217827245711364));
#15849=CARTESIAN_POINT('',(-0.0385114728776262,0.00969116769071119,-0.0217922854079731));
#15850=CARTESIAN_POINT('',(-0.0385114732742117,0.00969116834084262,-0.0217922858702222));
#15851=CARTESIAN_POINT('',(-0.0385114736704593,0.0140270890746655,-0.019288941705194));
#15852=CARTESIAN_POINT('',(-0.0385114736704593,0.012674860590309,-0.020272294223402));
#15853=CARTESIAN_POINT('',(-0.0385114736704593,0.0112188914949441,-0.0211128983725261));
#15854=CARTESIAN_POINT('',(-0.0385114736704593,0.00969116899111081,-0.0217922863325698));
#15855=CARTESIAN_POINT('',(-0.0385114728778453,0.0140270889245788,-0.0192889401165226));
#15856=CARTESIAN_POINT('',(-0.0385114728777164,0.0140270889245852,-0.0192889401165866));
#15857=CARTESIAN_POINT('',(-0.0385033092139972,0.0140254585383594,-0.0192726423546479));
#15858=CARTESIAN_POINT('',(-0.0384948822128803,0.0140225270456425,-0.0192567216305467));
#15859=CARTESIAN_POINT('',(-0.0384862032527859,0.0140183576393019,-0.0192411603786139));
#15860=CARTESIAN_POINT('',(-0.0361231220777228,0.00770660176395194,-0.0181444388314769));
#15861=CARTESIAN_POINT('',(-0.0364648722135284,0.00787297362658244,-0.0187168829308698));
#15862=CARTESIAN_POINT('',(-0.0370051857100642,0.00845252547520145,-0.019493059608721));
#15863=CARTESIAN_POINT('',(-0.0375391602638124,0.00968559833622874,-0.0199436995216774));
#15864=CARTESIAN_POINT('',(-0.0377837871637064,0.0107243093220201,-0.0198906462410908));
#15865=CARTESIAN_POINT('',(-0.0378106634033261,0.0116810478206927,-0.0193992046145791));
#15866=CARTESIAN_POINT('',(-0.0375458092115704,0.0125508820226309,-0.0183019088978515));
#15867=CARTESIAN_POINT('',(-0.0370936280807999,0.0126082281033858,-0.0172854180292052));
#15868=CARTESIAN_POINT('',(-0.0367610930019189,0.0124258527783243,-0.0167032268933286));
#15869=CARTESIAN_POINT('',(-0.0367610930181501,0.0124258527913459,-0.0167032269172659));
#15870=CARTESIAN_POINT('',(-0.0361231220786324,0.00770660176472532,-0.0181444388312368));
#15871=CARTESIAN_POINT('',(-0.0367610930019189,0.0124258527783243,-0.0167032268933286));
#15872=CARTESIAN_POINT('',(-0.0364268270990884,0.0122425282637756,-0.016118005443108));
#15873=CARTESIAN_POINT('',(-0.0358828098136817,0.0116542707196792,-0.0153834168354138));
#15874=CARTESIAN_POINT('',(-0.0352742106702343,0.0104542679403436,-0.0149560441847424));
#15875=CARTESIAN_POINT('',(-0.034970034410582,0.00942843977547389,-0.0150102461084905));
#15876=CARTESIAN_POINT('',(-0.0349337878900483,0.00847535144861393,-0.0154977244593865));
#15877=CARTESIAN_POINT('',(-0.0351821444489868,0.00782363555287664,-0.0163099017911));
#15878=CARTESIAN_POINT('',(-0.0356144093597047,0.00756137032066298,-0.0172491749161208));
#15879=CARTESIAN_POINT('',(-0.0359478246821774,0.00762126293631469,-0.0178508092217905));
#15880=CARTESIAN_POINT('',(-0.0361231220777228,0.00770660176395194,-0.0181444388314769));
#15881=CARTESIAN_POINT('',(-0.0247416697501165,0.,-9.27109177476128E-16));
#15882=CARTESIAN_POINT('',(-0.038486203260216,0.0236725124984624,-0.002519673636394));
#15883=CARTESIAN_POINT('',(-0.0384948821067245,0.0236880734374344,-0.00251550387707458));
#15884=CARTESIAN_POINT('',(-0.0385033089939486,0.0237033267480975,-0.00251008235773586));
#15885=CARTESIAN_POINT('',(-0.0385114725590369,0.023718256032576,-0.00250334555419547));
#15886=CARTESIAN_POINT('',(-0.0385114731149663,0.0237182570487454,-0.00250334509564679));
#15887=CARTESIAN_POINT('',(-0.0385114736704593,0.,-9.39994586434264E-16));
#15888=CARTESIAN_POINT('',(-0.0385114718743307,0.0237182547802193,0.00250334611931137));
#15889=CARTESIAN_POINT('',(-0.0385114711901184,0.0237182535297626,0.00250334668357001));
#15890=CARTESIAN_POINT('',(-0.0385038414966823,0.0237043005914817,0.0025096427595367));
#15891=CARTESIAN_POINT('',(-0.0384954181831038,0.0236890346032608,0.00251524655040276));
#15892=CARTESIAN_POINT('',(-0.0384862012493829,0.0236725089103646,0.00251967460880542));
#15893=CARTESIAN_POINT('',(-0.0384862012657654,0.0236725088091823,0.00251967463590271));
#15894=CARTESIAN_POINT('',(-0.0384862012074146,0.0236725088385615,0.00251967462801615));
#15895=CARTESIAN_POINT('',(-0.0370999081087009,0.0211869262660569,0.00318568447108093));
#15896=CARTESIAN_POINT('',(-0.0357332398658379,0.0186914615155662,0.00385434223575671));
#15897=CARTESIAN_POINT('',(-0.0344330129923926,0.0161625399365206,0.00453196473062564));
#15898=CARTESIAN_POINT('',(-0.0361231220777228,0.0195668458469756,-0.0023981065151534));
#15899=CARTESIAN_POINT('',(-0.0364648722136017,0.0201457829107077,-0.00254024630548127));
#15900=CARTESIAN_POINT('',(-0.0370051857100481,0.0211077475601334,-0.00242642797910508));
#15901=CARTESIAN_POINT('',(-0.0375391602638148,0.0221145495981621,-0.0015838755607176));
#15902=CARTESIAN_POINT('',(-0.0377837871637081,0.0225879596037126,-0.000657798821766451));
#15903=CARTESIAN_POINT('',(-0.0378106634033168,0.0226407279192869,0.000416481880123052));
#15904=CARTESIAN_POINT('',(-0.0375458092116211,0.022125359054538,0.00171842820318643));
#15905=CARTESIAN_POINT('',(-0.0370936280805749,0.0212737251842116,0.00227633678167192));
#15906=CARTESIAN_POINT('',(-0.0367610930019189,0.0206783452020235,0.00240949073966257));
#15907=CARTESIAN_POINT('',(-0.0367610930181502,0.0206783452308322,0.00240949072780955));
#15908=CARTESIAN_POINT('',(-0.0361231220786325,0.0195668458477632,-0.00239810651169203));
#15909=CARTESIAN_POINT('',(-0.0367610930019189,0.0206783452020235,0.00240949073966257));
#15910=CARTESIAN_POINT('',(-0.03642682709907,0.0200798663083023,0.00254333772243173));
#15911=CARTESIAN_POINT('',(-0.035882809813686,0.019149565135917,0.00240118609225308));
#15912=CARTESIAN_POINT('',(-0.0352742106702333,0.0181794481747533,0.00157563951687282));
#15913=CARTESIAN_POINT('',(-0.0349700344105827,0.0177134743348323,0.000660145306282492));
#15914=CARTESIAN_POINT('',(-0.0349337878900463,0.0176590988069142,-0.000408992572770604));
#15915=CARTESIAN_POINT('',(-0.0351821444489944,0.0180366070604978,-0.00137948376032849));
#15916=CARTESIAN_POINT('',(-0.0356144093596766,0.0187189088315577,-0.00207624867662167));
#15917=CARTESIAN_POINT('',(-0.035947824682238,0.0192698857319822,-0.00232519730293998));
#15918=CARTESIAN_POINT('',(-0.0361231220777228,0.0195668458469756,-0.0023981065151534));
#15919=CARTESIAN_POINT('',(-0.039226004293684,0.0197767818485,0.003563531529));
#15920=CARTESIAN_POINT('',(-0.0442,0.023672508708,0.002519674663));
#15921=CARTESIAN_POINT('',(-0.0422954004219218,0.023672508708,0.002519674663));
#15922=CARTESIAN_POINT('',(-0.0403908008438436,0.023672508708,0.002519674663));
#15923=CARTESIAN_POINT('',(-0.0384862012657654,0.023672508708,0.002519674663));
#15924=CARTESIAN_POINT('',(-0.0247416697501165,0.,-9.27109177476128E-16));
#15925=CARTESIAN_POINT('',(-0.0384862032593478,0.0140183576289848,0.0192411603767344));
#15926=CARTESIAN_POINT('',(-0.0384948822191775,0.0140225270354065,0.0192567216280387));
#15927=CARTESIAN_POINT('',(-0.038503309213364,0.0140254585381575,0.0192726423534367));
#15928=CARTESIAN_POINT('',(-0.0385114728769827,0.0140270889244387,0.01928894011512));
#15929=CARTESIAN_POINT('',(-0.0385114732738496,0.0140270890035019,0.0192889409072152));
#15930=CARTESIAN_POINT('',(-0.0385114736704593,0.00969116897825783,0.0217922863382837));
#15931=CARTESIAN_POINT('',(-0.0385114736704593,0.011218891489756,0.0211128983759107));
#15932=CARTESIAN_POINT('',(-0.0385114736704593,0.0126748605921952,0.0202722942228765));
#15933=CARTESIAN_POINT('',(-0.0385114736704593,0.014027089082578,0.0192889416994381));
#15934=CARTESIAN_POINT('',(-0.0385114720962522,0.00969116641671853,0.0217922844930147));
#15935=CARTESIAN_POINT('',(-0.0385114717024072,0.00969116577635566,0.0217922840319173));
#15936=CARTESIAN_POINT('',(-0.0385033084027854,0.00967786742257547,0.0217827235606114));
#15937=CARTESIAN_POINT('',(-0.038494881794112,0.00966554605324076,0.0217722249123752));
#15938=CARTESIAN_POINT('',(-0.0384862032527165,0.00965415486648457,0.0217608340241601));
#15939=CARTESIAN_POINT('',(-0.0361231220777228,0.0118602440896865,0.015746332315506));
#15940=CARTESIAN_POINT('',(-0.0364648722136085,0.0122728092489834,0.0161766366562693));
#15941=CARTESIAN_POINT('',(-0.0370051857103236,0.0126552220632647,0.0170666316051076));
#15942=CARTESIAN_POINT('',(-0.0375391602633533,0.0124289512728845,0.0183598239629085));
#15943=CARTESIAN_POINT('',(-0.0377837871654629,0.0118636502964869,0.0192328474262822));
#15944=CARTESIAN_POINT('',(-0.0378106633967592,0.0109596800744716,0.0198156864636229));
#15945=CARTESIAN_POINT('',(-0.0375458092464411,0.00957447705560089,0.0200203371759163));
#15946=CARTESIAN_POINT('',(-0.0370936279261474,0.00866549692365674,0.0195617546232574));
#15947=CARTESIAN_POINT('',(-0.036761093001919,0.00825249241403732,0.0191127176213848));
#15948=CARTESIAN_POINT('',(-0.0367610930181502,0.00825249243626566,0.0191127176418733));
#15949=CARTESIAN_POINT('',(-0.0361231220786325,0.0118602440845922,0.0157463323192722));
#15950=CARTESIAN_POINT('',(-0.036761093001919,0.00825249241403732,0.0191127176213848));
#15951=CARTESIAN_POINT('',(-0.036426827099111,0.00783733807984076,0.0186613431873148));
#15952=CARTESIAN_POINT('',(-0.035882809813574,0.00749529443304704,0.0177846029157222));
#15953=CARTESIAN_POINT('',(-0.0352742106704064,0.00772518021396054,0.0165316837164498));
#15954=CARTESIAN_POINT('',(-0.0349700344099314,0.00828503457162375,0.0156703914105354));
#15955=CARTESIAN_POINT('',(-0.0349337878924788,0.00918374736601869,0.0150887318900222));
#15956=CARTESIAN_POINT('',(-0.0351821444399159,0.0102129715007087,0.0149304180205763));
#15957=CARTESIAN_POINT('',(-0.035614409393558,0.0111575385677808,0.015172926274143));
#15958=CARTESIAN_POINT('',(-0.0359478246092337,0.0116486226930708,0.0155256118420533));
#15959=CARTESIAN_POINT('',(-0.0361231220777228,0.0118602440896865,0.015746332315506));
#15960=CARTESIAN_POINT('',(-0.0247416697501165,0.,-9.27109177476128E-16));
#15961=CARTESIAN_POINT('',(-0.0384862032593708,-0.0096541548701199,0.0217608340143427));
#15962=CARTESIAN_POINT('',(-0.0384948821046016,-0.00966554645544961,0.0217722253014528));
#15963=CARTESIAN_POINT('',(-0.0385033089913836,-0.00967786828270555,0.0217827242938166));
#15964=CARTESIAN_POINT('',(-0.0385114725553467,-0.0096911671656983,0.0217922850305355));
#15965=CARTESIAN_POINT('',(-0.0385114731130998,-0.00969116807390871,0.0217922856835205));
#15966=CARTESIAN_POINT('',(-0.0385114736704593,-0.0140270890860421,0.0192889416969189));
#15967=CARTESIAN_POINT('',(-0.0385114736704593,-0.0126748605958359,0.0202722942206002));
#15968=CARTESIAN_POINT('',(-0.0385114736704593,-0.0112188914935475,0.021112898373896));
#15969=CARTESIAN_POINT('',(-0.0385114736704593,-0.00969116898217136,0.0217922863365434));
#15970=CARTESIAN_POINT('',(-0.0385114728767313,-0.0140270889243563,0.0192889401142976));
#15971=CARTESIAN_POINT('',(-0.0385114728763616,-0.0140270889247215,0.0192889401144462));
#15972=CARTESIAN_POINT('',(-0.0385033092129711,-0.014025458538453,0.019272642353242));
#15973=CARTESIAN_POINT('',(-0.0384948822124526,-0.0140225270454405,0.0192567216297753));
#15974=CARTESIAN_POINT('',(-0.0384862032527417,-0.0140183576392802,0.019241160378533));
#15975=CARTESIAN_POINT('',(-0.0361231220777228,-0.00770660175650897,0.0181444388346364));
#15976=CARTESIAN_POINT('',(-0.0364648722136209,-0.00787297366731662,0.0187168829137092));
#15977=CARTESIAN_POINT('',(-0.0370051857103217,-0.00845252549508946,0.0194930596000144));
#15978=CARTESIAN_POINT('',(-0.0375391602633525,-0.00968559832410782,0.019943699526334));
#15979=CARTESIAN_POINT('',(-0.0377837871654679,-0.0107243093096923,0.0198906462517043));
#15980=CARTESIAN_POINT('',(-0.03781066339674,-0.0116810478333493,0.0193992045938186));
#15981=CARTESIAN_POINT('',(-0.0375458092465435,-0.0125508820586186,0.018301908946452));
#15982=CARTESIAN_POINT('',(-0.0370936279256935,-0.0126082279839681,0.0172854177833506));
#15983=CARTESIAN_POINT('',(-0.036761093001919,-0.0124258527881758,0.016703226885998));
#15984=CARTESIAN_POINT('',(-0.0367610930181502,-0.0124258527946297,0.0167032269148224));
#15985=CARTESIAN_POINT('',(-0.0361231220786325,-0.00770660176224433,0.01814443883229));
#15986=CARTESIAN_POINT('',(-0.036761093001919,-0.0124258527881758,0.016703226885998));
#15987=CARTESIAN_POINT('',(-0.0364268270991507,-0.0122425282287825,0.0161180054691239));
#15988=CARTESIAN_POINT('',(-0.0358828098135649,-0.0116542707355394,0.0153834168229345));
#15989=CARTESIAN_POINT('',(-0.0352742106704084,-0.0104542679526858,0.014956044176835));
#15990=CARTESIAN_POINT('',(-0.0349700344099297,-0.00942843976427119,0.015010246114524));
#15991=CARTESIAN_POINT('',(-0.0349337878924834,-0.00847535144396104,0.0154977244663839));
#15992=CARTESIAN_POINT('',(-0.0351821444398992,-0.00782363554441411,0.0163099017780492));
#15993=CARTESIAN_POINT('',(-0.0356144093936205,-0.00756137031897134,0.0172491749807311));
#15994=CARTESIAN_POINT('',(-0.035947824609099,-0.00762126291761072,0.0178508090922294));
#15995=CARTESIAN_POINT('',(-0.0361231220777228,-0.00770660175650897,0.0181444388346364));
#15996=CARTESIAN_POINT('',(-0.0247416697501165,0.,-9.27109177476128E-16));
#15997=CARTESIAN_POINT('',(-0.0384862032581869,-0.0236725124992893,0.00251967363853479));
#15998=CARTESIAN_POINT('',(-0.0384948822179627,-0.0236880736413488,0.0025155038247818));
#15999=CARTESIAN_POINT('',(-0.0385033092129298,-0.0237033271444534,0.00251008221703059));
#16000=CARTESIAN_POINT('',(-0.038511472876488,-0.0237182566131209,0.00250334529222524));
#16001=CARTESIAN_POINT('',(-0.0385114732736763,-0.02371825733873,0.00250334496717108));
#16002=CARTESIAN_POINT('',(-0.0385114736704593,-0.0237182580651627,-0.00250334463653795));
#16003=CARTESIAN_POINT('',(-0.0385114736704593,-0.0238937520861163,-0.000840604150423141));
#16004=CARTESIAN_POINT('',(-0.0385114736704593,-0.0238937520859224,0.00084060415593165));
#16005=CARTESIAN_POINT('',(-0.0385114736704593,-0.0237182580645854,0.00250334464200599));
#16006=CARTESIAN_POINT('',(-0.0385114728771051,-0.0237182566137558,-0.0025033452919386));
#16007=CARTESIAN_POINT('',(-0.0385114728771736,-0.0237182566135553,-0.00250334529157726));
#16008=CARTESIAN_POINT('',(-0.0385033092137543,-0.0237033271451377,-0.00251008221630948));
#16009=CARTESIAN_POINT('',(-0.0384948822126514,-0.0236880736481024,-0.00251550383130167));
#16010=CARTESIAN_POINT('',(-0.038486203252893,-0.0236725125060437,-0.00251967364531955));
#16011=CARTESIAN_POINT('',(-0.0361231220777228,-0.01956684584839,0.00239810650361112));
#16012=CARTESIAN_POINT('',(-0.0364648722135854,-0.0201457829121783,0.00254024629359048));
#16013=CARTESIAN_POINT('',(-0.0370051857097729,-0.0211077475580505,0.00242642799183558));
#16014=CARTESIAN_POINT('',(-0.0375391602642789,-0.0221145495984874,0.00158387556971517));
#16015=CARTESIAN_POINT('',(-0.0377837871619422,-0.0225879596001145,0.000657798828281427));
#16016=CARTESIAN_POINT('',(-0.0378106634099163,-0.0226407279317958,-0.000416481859769928));
#16017=CARTESIAN_POINT('',(-0.0375458091765785,-0.0221253589897648,-0.00171842825316367));
#16018=CARTESIAN_POINT('',(-0.0370936282359893,-0.0212737254634035,-0.00227633671071596));
#16019=CARTESIAN_POINT('',(-0.0367610930019189,-0.0206783452030119,-0.00240949073118205));
#16020=CARTESIAN_POINT('',(-0.0367610930181502,-0.0206783452311617,-0.00240949072498272));
#16021=CARTESIAN_POINT('',(-0.0361231220786325,-0.0195668458482347,0.00239810650784461));
#16022=CARTESIAN_POINT('',(-0.0367610930019189,-0.0206783452030119,-0.00240949073118205));
#16023=CARTESIAN_POINT('',(-0.0364268270992314,-0.0200798663096345,-0.00254333771413222));
#16024=CARTESIAN_POINT('',(-0.0358828098134473,-0.0191495651337216,-0.00240118610461706));
#16025=CARTESIAN_POINT('',(-0.0352742106705773,-0.0181794481741787,-0.00157563953253189));
#16026=CARTESIAN_POINT('',(-0.0349700344092999,-0.0177134743335201,-0.000660145294956659));
#16027=CARTESIAN_POINT('',(-0.0349337878948338,-0.0176590988142993,0.000408992586881077));
#16028=CARTESIAN_POINT('',(-0.035182144431127,-0.0180366070313037,0.00137948373618994));
#16029=CARTESIAN_POINT('',(-0.0356144094263585,-0.0187189089456695,0.0020762486950472));
#16030=CARTESIAN_POINT('',(-0.0359478245385584,-0.0192698854899551,0.00232519723181412));
#16031=CARTESIAN_POINT('',(-0.0361231220777228,-0.01956684584839,0.00239810650361112));
#16032=CARTESIAN_POINT('',(-0.0247416697501165,0.,-9.27109177476128E-16));
#16033=CARTESIAN_POINT('',(-0.038486203252956,-0.0140183576393836,-0.0192411603789189));
#16034=CARTESIAN_POINT('',(-0.0384948822124652,-0.0140225270454284,-0.019256721629813));
#16035=CARTESIAN_POINT('',(-0.0385033092130316,-0.0140254585380152,-0.0192726423528298));
#16036=CARTESIAN_POINT('',(-0.0385114728762402,-0.0140270889242906,-0.0192889401136396));
#16037=CARTESIAN_POINT('',(-0.0385114732734456,-0.0140270890073774,-0.0192889409035327));
#16038=CARTESIAN_POINT('',(-0.0385114736704593,-0.0096911689871971,-0.0217922863343103));
#16039=CARTESIAN_POINT('',(-0.0385114736704593,-0.0112188914984166,-0.0211128983713105));
#16040=CARTESIAN_POINT('',(-0.0385114736704593,-0.0126748606005111,-0.020272294217679));
#16041=CARTESIAN_POINT('',(-0.0385114736704593,-0.0140270890904905,-0.0192889416936859));
#16042=CARTESIAN_POINT('',(-0.0385114728774152,-0.00969116769002384,-0.0217922854074788));
#16043=CARTESIAN_POINT('',(-0.0385114728772461,-0.00969116769009225,-0.021792285407528));
#16044=CARTESIAN_POINT('',(-0.038503309213807,-0.00967786860783287,-0.0217827245709812));
#16045=CARTESIAN_POINT('',(-0.038494882212988,-0.00966554660309386,-0.0217722254621444));
#16046=CARTESIAN_POINT('',(-0.0384862032532088,-0.00965415486713206,-0.0217608340248075));
#16047=CARTESIAN_POINT('',(-0.0361231220777228,-0.0118602440803994,-0.015746332322503));
#16048=CARTESIAN_POINT('',(-0.036464872213627,-0.0122728092814391,-0.0161766366319176));
#16049=CARTESIAN_POINT('',(-0.0370051857100415,-0.0126552220776526,-0.01706663159448));
#16050=CARTESIAN_POINT('',(-0.0375391602638173,-0.0124289512594974,-0.0183598239733153));
#16051=CARTESIAN_POINT('',(-0.0377837871637024,-0.0118636502776772,-0.0192328474337847));
#16052=CARTESIAN_POINT('',(-0.0378106634033369,-0.0109596800952083,-0.019815686465));
#16053=CARTESIAN_POINT('',(-0.0375458092115145,-0.00957447702796622,-0.0200203371222328));
#16054=CARTESIAN_POINT('',(-0.037093628081047,-0.0086654970730925,-0.0195617548508813));
#16055=CARTESIAN_POINT('',(-0.0367610930019189,-0.00825249242187748,-0.0191127176180015));
#16056=CARTESIAN_POINT('',(-0.0367610930181501,-0.00825249243887905,-0.0191127176407455));
#16057=CARTESIAN_POINT('',(-0.0361231220786324,-0.0118602440814965,-0.0157463323216046));
#16058=CARTESIAN_POINT('',(-0.0367610930019189,-0.00825249242187748,-0.0191127176180015));
#16059=CARTESIAN_POINT('',(-0.0364268270990136,-0.00783733803641719,-0.018661343205973));
#16060=CARTESIAN_POINT('',(-0.0358828098136985,-0.00749529441315766,-0.017784602925027));
#16061=CARTESIAN_POINT('',(-0.0352742106702312,-0.00772518023068291,-0.016531683708193));
#16062=CARTESIAN_POINT('',(-0.0349700344105825,-0.00828503455619132,-0.0156703914194872));
#16063=CARTESIAN_POINT('',(-0.0349337878900495,-0.00918374735540738,-0.0150887318920016));
#16064=CARTESIAN_POINT('',(-0.0351821444489816,-0.0102129715049413,-0.0149304180362941));
#16065=CARTESIAN_POINT('',(-0.0356144093597242,-0.0111575385083902,-0.0151729262453948));
#16066=CARTESIAN_POINT('',(-0.0359478246821352,-0.0116486227929187,-0.0155256119249019));
#16067=CARTESIAN_POINT('',(-0.0361231220777228,-0.0118602440803994,-0.015746332322503));
#16068=CARTESIAN_POINT('',(-0.0345,0.01,-0.017320508076));
#16069=CARTESIAN_POINT('',(-0.0370209006250624,0.0120502416069907,-0.0166731987585513));
#16070=CARTESIAN_POINT('',(-0.0369382714896785,0.0120102199855764,-0.016546437114325));
#16071=CARTESIAN_POINT('',(-0.0368384384344523,0.0119515655400817,-0.0164007187842568));
#16072=CARTESIAN_POINT('',(-0.0367214014593838,0.0118619547328937,-0.0162455082750017));
#16073=CARTESIAN_POINT('',(-0.0367214015196458,0.0118619576137187,-0.0162455065980668));
#16074=CARTESIAN_POINT('',(-0.037020900637956,0.0120502416154678,-0.0166731987850141));
#16075=CARTESIAN_POINT('',(-0.0367214013837088,0.0118619546747634,-0.0162455081743171));
#16076=CARTESIAN_POINT('',(-0.0367099515900364,0.0118531879996303,-0.0162303238457225));
#16077=CARTESIAN_POINT('',(-0.036670659517387,0.0118230656559306,-0.0161785319977277));
#16078=CARTESIAN_POINT('',(-0.036581771380862,0.0117478247863627,-0.0160659297891458));
#16079=CARTESIAN_POINT('',(-0.0364479212855715,0.0116231137497877,-0.0159049183945184));
#16080=CARTESIAN_POINT('',(-0.0363510261528849,0.0115197512730407,-0.0157983752279772));
#16081=CARTESIAN_POINT('',(-0.0362580223097223,0.011416510277242,-0.0156993012950561));
#16082=CARTESIAN_POINT('',(-0.0361233029084067,0.0112500261099531,-0.0155680128195404));
#16083=CARTESIAN_POINT('',(-0.0360272431295662,0.0111204292982917,-0.0154825522935279));
#16084=CARTESIAN_POINT('',(-0.0359036001279196,0.0109384060206373,-0.0153831278620205));
#16085=CARTESIAN_POINT('',(-0.0357761189415156,0.0107336230397511,-0.0152928731905691));
#16086=CARTESIAN_POINT('',(-0.0355839197980515,0.0103729533951222,-0.0151906973984985));
#16087=CARTESIAN_POINT('',(-0.0354386203310907,0.0100314764218445,-0.0151589427817623));
#16088=CARTESIAN_POINT('',(-0.0352978141924959,0.00958374411058124,-0.015196844402381));
#16089=CARTESIAN_POINT('',(-0.0352031355092724,0.00907592308678395,-0.0153447793638773));
#16090=CARTESIAN_POINT('',(-0.0352317165648889,0.00855567326232278,-0.0156889692127796));
#16091=CARTESIAN_POINT('',(-0.0353617578831115,0.00822759558954855,-0.0160791452283518));
#16092=CARTESIAN_POINT('',(-0.0355339605712917,0.00801012797788875,-0.0164765050992009));
#16093=CARTESIAN_POINT('',(-0.0356900432181194,0.007905672438546,-0.0167851632512574));
#16094=CARTESIAN_POINT('',(-0.0358977301719722,0.00785023330030782,-0.0171562408689187));
#16095=CARTESIAN_POINT('',(-0.0360269463636352,0.0078480581130412,-0.0173712503755659));
#16096=CARTESIAN_POINT('',(-0.0361556833141385,0.00786282854433334,-0.0175781112950878));
#16097=CARTESIAN_POINT('',(-0.0362517163778589,0.00788664178093596,-0.0177265531559471));
#16098=CARTESIAN_POINT('',(-0.036337936705,0.00791668749714797,-0.0178562799663004));
#16099=CARTESIAN_POINT('',(-0.0363829297000817,0.00793596622153825,-0.0179223922516189));
#16100=CARTESIAN_POINT('',(-0.0363829296981285,0.00793596622218309,-0.0179223922530286));
#16101=CARTESIAN_POINT('',(-0.0363829297000817,0.00793596622153825,-0.0179223922516189));
#16102=CARTESIAN_POINT('',(-0.0364957535948001,0.00798408903520211,-0.018087419206871));
#16103=CARTESIAN_POINT('',(-0.0366085774895185,0.0080520952982146,-0.0182466381820913));
#16104=CARTESIAN_POINT('',(-0.0367214013842369,0.00813804543863112,-0.018395508174088));
#16105=CARTESIAN_POINT('',(-0.0367214014146636,0.00813803958835936,-0.0183955115197437));
#16106=CARTESIAN_POINT('',(-0.0367214014593838,0.00813804549645274,-0.0183955082742379));
#16107=CARTESIAN_POINT('',(-0.0368094504194448,0.00820546129493275,-0.0185122758337192));
#16108=CARTESIAN_POINT('',(-0.0369082047152564,0.00829303764241074,-0.0186381460995257));
#16109=CARTESIAN_POINT('',(-0.0370729160017973,0.00846997363213822,-0.0188345415471286));
#16110=CARTESIAN_POINT('',(-0.0372054092113008,0.00862943751340597,-0.0189847044560509));
#16111=CARTESIAN_POINT('',(-0.0374076931229372,0.00892027604482932,-0.0191924775219796));
#16112=CARTESIAN_POINT('',(-0.0375741836148829,0.00921705183109107,-0.0193348076621258));
#16113=CARTESIAN_POINT('',(-0.0377619138370971,0.00963575500054258,-0.0194525344836347));
#16114=CARTESIAN_POINT('',(-0.037887321460399,0.0100037924316706,-0.019482814463935));
#16115=CARTESIAN_POINT('',(-0.0379943792822189,0.0104428423755329,-0.0194389153257726));
#16116=CARTESIAN_POINT('',(-0.0380653382950535,0.0109633665553823,-0.0192778414401676));
#16117=CARTESIAN_POINT('',(-0.0380390815294276,0.0114596043683887,-0.0189394219781793));
#16118=CARTESIAN_POINT('',(-0.0379290145681861,0.0117932120462459,-0.0185312244554124));
#16119=CARTESIAN_POINT('',(-0.0377914075938047,0.0119983498352797,-0.0181451935333134));
#16120=CARTESIAN_POINT('',(-0.0376479878673514,0.0121064916090377,-0.0178074586875425));
#16121=CARTESIAN_POINT('',(-0.0374402992000161,0.0121604331951634,-0.0173824655935396));
#16122=CARTESIAN_POINT('',(-0.0372619157421967,0.0121430293601063,-0.0170606765916029));
#16123=CARTESIAN_POINT('',(-0.0371044376010776,0.0120907029448459,-0.0168013531294359));
#16124=CARTESIAN_POINT('',(-0.0370209006250624,0.0120502416069907,-0.0166731987585513));
#16125=CARTESIAN_POINT('',(-0.0345,0.02,0.));
#16126=CARTESIAN_POINT('',(-0.0370209006250623,0.0204645344905706,0.0020992159743748));
#16127=CARTESIAN_POINT('',(-0.0369382705057487,0.0203347433302252,0.00212793739765262));
#16128=CARTESIAN_POINT('',(-0.0368384374592961,0.0201792202695511,0.00214999998707071));
#16129=CARTESIAN_POINT('',(-0.0367214014857045,0.0200000001551052,0.00214999999999999));
#16130=CARTESIAN_POINT('',(-0.0367214015239592,0.020000000186686,0.00215000333369359));
#16131=CARTESIAN_POINT('',(-0.037020900637956,0.020464534518328,0.00209921596804585));
#16132=CARTESIAN_POINT('',(-0.0367214013837088,0.02,0.00215));
#16133=CARTESIAN_POINT('',(-0.0367099554160874,0.0199824725070566,0.00215));
#16134=CARTESIAN_POINT('',(-0.0366706659873135,0.019922562352937,0.00214980948896017));
#16135=CARTESIAN_POINT('',(-0.0365817765395305,0.0197874235171236,0.00214095075204637));
#16136=CARTESIAN_POINT('',(-0.0364479182980935,0.0195856157382105,0.0021134520269105));
#16137=CARTESIAN_POINT('',(-0.036351027246845,0.0194416715666082,0.00207720991389666));
#16138=CARTESIAN_POINT('',(-0.0362580217381144,0.0193042480471294,0.00203733687752704));
#16139=CARTESIAN_POINT('',(-0.0361233041008781,0.0191073093362409,0.0019588033066822));
#16140=CARTESIAN_POINT('',(-0.0360272389301111,0.0189684923098096,0.00188929327715607));
#16141=CARTESIAN_POINT('',(-0.0359036157332686,0.018791404597601,0.00178139164708577));
#16142=CARTESIAN_POINT('',(-0.0357760361093145,0.0186107110588261,0.00164905760404357));
#16143=CARTESIAN_POINT('',(-0.0355845872611166,0.0183429504643919,0.00138866627066025));
#16144=CARTESIAN_POINT('',(-0.0354400098074399,0.0181456531209698,0.00111147707696002));
#16145=CARTESIAN_POINT('',(-0.03529745132709,0.0179522358157694,0.000700457148034725));
#16146=CARTESIAN_POINT('',(-0.0352033477140133,0.0178272165772559,0.00018810871030881));
#16147=CARTESIAN_POINT('',(-0.0352316825933261,0.0178648366965161,-0.000435137210319832));
#16148=CARTESIAN_POINT('',(-0.0353617642821612,0.0180387546663257,-0.000914250187794874));
#16149=CARTESIAN_POINT('',(-0.0355339588539763,0.018274133653175,-0.00130128242879006));
#16150=CARTESIAN_POINT('',(-0.0356900436883312,0.0184892146354852,-0.0015460673103522));
#16151=CARTESIAN_POINT('',(-0.0358977301136426,0.0187828569969928,-0.00177961911331699));
#16152=CARTESIAN_POINT('',(-0.0360269463745861,0.018967973191657,-0.00188900746452468));
#16153=CARTESIAN_POINT('',(-0.0361556833111519,0.0191545051998489,-0.00197964638969947));
#16154=CARTESIAN_POINT('',(-0.0362517163788544,0.0192949662460383,-0.00203324444307963));
#16155=CARTESIAN_POINT('',(-0.0363379367050664,0.0194223358162089,-0.00207208749676157));
#16156=CARTESIAN_POINT('',(-0.0363829297000817,0.0194892300968965,-0.00208844777432515));
#16157=CARTESIAN_POINT('',(-0.0363829296981285,0.0194892300988016,-0.00208844777506104));
#16158=CARTESIAN_POINT('',(-0.0363829297000817,0.0194892300968965,-0.00208844777432515));
#16159=CARTESIAN_POINT('',(-0.0364957535948001,0.0196562090392939,-0.00212928567282428));
#16160=CARTESIAN_POINT('',(-0.0366085774895185,0.0198280998481142,-0.00215000000905572));
#16161=CARTESIAN_POINT('',(-0.0367214013842369,0.0200000001132622,-0.00215));
#16162=CARTESIAN_POINT('',(-0.0367214014146637,0.0200000000856372,-0.00215000673932028));
#16163=CARTESIAN_POINT('',(-0.0367214014593838,0.0200000002289055,-0.00214999999999999));
#16164=CARTESIAN_POINT('',(-0.0368094504193861,0.0201348318009116,-0.00214999998564479));
#16165=CARTESIAN_POINT('',(-0.0369082047152033,0.0202876268224398,-0.0021370917768919));
#16166=CARTESIAN_POINT('',(-0.0370729160019053,0.0205461782643721,-0.00208205843868064));
#16167=CARTESIAN_POINT('',(-0.0372054092112306,0.020755955098582,-0.00201904012105865));
#16168=CARTESIAN_POINT('',(-0.0374076931230288,0.0210813111179108,-0.00187105309729519));
#16169=CARTESIAN_POINT('',(-0.0375741836148664,0.0213529605279511,-0.00168520279732712));
#16170=CARTESIAN_POINT('',(-0.0377619138370714,0.0216642665308313,-0.00138145862673429));
#16171=CARTESIAN_POINT('',(-0.0378873214604069,0.0218745084786354,-0.00107786885189048));
#16172=CARTESIAN_POINT('',(-0.0379943792822128,0.0220560156817041,-0.000675690877956248));
#16173=CARTESIAN_POINT('',(-0.0380653382950567,0.0221767836948601,-0.000144366772012301));
#16174=CARTESIAN_POINT('',(-0.0380390815294298,0.0221318227501571,0.000454597511353307));
#16175=CARTESIAN_POINT('',(-0.0379290145681815,0.0219451171645996,0.000947608996721526));
#16176=CARTESIAN_POINT('',(-0.0377914075938135,0.0217133734739575,0.00131827899434535));
#16177=CARTESIAN_POINT('',(-0.0376479878673206,0.0214749574045774,0.00158079994060532));
#16178=CARTESIAN_POINT('',(-0.0374402992000349,0.021133873381878,0.00184001127146523));
#16179=CARTESIAN_POINT('',(-0.0372619157421523,0.0208464940139058,0.00198583360922132));
#16180=CARTESIAN_POINT('',(-0.0371044376010594,0.020595750100268,0.00207017933538683));
#16181=CARTESIAN_POINT('',(-0.0370209006250624,0.0204645344905706,0.0020992159743748));
#16182=CARTESIAN_POINT('',(-0.0345,0.01,0.017320508076));
#16183=CARTESIAN_POINT('',(-0.0367214013837088,0.00813804543876341,0.0183955081743171));
#16184=CARTESIAN_POINT('',(-0.036709951590334,0.0081292787622546,0.0183803238470431));
#16185=CARTESIAN_POINT('',(-0.0366706595167616,0.00809948687850548,0.0183283412064286));
#16186=CARTESIAN_POINT('',(-0.0365817713831444,0.00803959093910059,0.0182068796030137));
#16187=CARTESIAN_POINT('',(-0.036447921275181,0.00796250650255608,0.0180183709572674));
#16188=CARTESIAN_POINT('',(-0.0363510262349874,0.00792191862466955,0.0178755850102194));
#16189=CARTESIAN_POINT('',(-0.0362580220091763,0.00788773869361132,0.0177366380281489));
#16190=CARTESIAN_POINT('',(-0.0361233040284883,0.00785728120029016,0.0175268168356142));
#16191=CARTESIAN_POINT('',(-0.0360272389494077,0.00784807019341441,0.0173718428777057));
#16192=CARTESIAN_POINT('',(-0.035903615728472,0.00785297187537506,0.017164529571628));
#16193=CARTESIAN_POINT('',(-0.0357760361120757,0.00787722975389325,0.0169418773656573));
#16194=CARTESIAN_POINT('',(-0.0355845872602483,0.00796885496384819,0.0165797942171482));
#16195=CARTESIAN_POINT('',(-0.0354400098076728,0.00811025917636308,0.0162703351102285));
#16196=CARTESIAN_POINT('',(-0.0352974513270266,0.00836950422341811,0.0158973208455679));
#16197=CARTESIAN_POINT('',(-0.0352033477140518,0.00875070136687583,0.0155328767903185));
#16198=CARTESIAN_POINT('',(-0.0352316825933103,0.0093092582264464,0.0152538338089243));
#16199=CARTESIAN_POINT('',(-0.0353617642821792,0.00981114122123326,0.015164894700211));
#16200=CARTESIAN_POINT('',(-0.0355339588539459,0.0102640104672661,0.0151752227618142));
#16201=CARTESIAN_POINT('',(-0.0356900436884346,0.0105835408845637,0.0152390959156379));
#16202=CARTESIAN_POINT('',(-0.0358977301136305,0.0109326238595562,0.015376621758773));
#16203=CARTESIAN_POINT('',(-0.0360269463745872,0.0111199150479226,0.0154822429103865));
#16204=CARTESIAN_POINT('',(-0.0361556833111771,0.0112916766638192,0.015598464905532));
#16205=CARTESIAN_POINT('',(-0.0362517163787524,0.0114083244625806,0.0156933087129476));
#16206=CARTESIAN_POINT('',(-0.0363379367050222,0.0115056483189857,0.0157841924695875));
#16207=CARTESIAN_POINT('',(-0.0363829297000817,0.0115532638753583,0.0158339444772937));
#16208=CARTESIAN_POINT('',(-0.0363829296981285,0.0115532638766184,0.0158339444786343));
#16209=CARTESIAN_POINT('',(-0.0367214015132256,0.0081380426038155,0.0183955099315374));
#16210=CARTESIAN_POINT('',(-0.0363829297000817,0.0115532638753583,0.0158339444772937));
#16211=CARTESIAN_POINT('',(-0.0364957535948001,0.0116721200040918,0.0159581335340468));
#16212=CARTESIAN_POINT('',(-0.0366085774895185,0.0117760045498996,0.0160966381730355));
#16213=CARTESIAN_POINT('',(-0.0367214013842369,0.0118619546746311,0.016245508174088));
#16214=CARTESIAN_POINT('',(-0.036721401387368,0.0118619604980822,0.0162455047799774));
#16215=CARTESIAN_POINT('',(-0.0367214014593838,0.0118619547324527,0.016245508274238));
#16216=CARTESIAN_POINT('',(-0.0368094504192976,0.0119293705059561,0.0163622758478791));
#16217=CARTESIAN_POINT('',(-0.036908204704608,0.0119945891381311,0.0165010543259075));
#16218=CARTESIAN_POINT('',(-0.0370729160195937,0.0120762047020714,0.0167524831030568));
#16219=CARTESIAN_POINT('',(-0.0372054091160399,0.0121265172076173,0.0169656643651337));
#16220=CARTESIAN_POINT('',(-0.0374076938913033,0.012161038121922,0.0173214241803676));
#16221=CARTESIAN_POINT('',(-0.0375741808104541,0.0121358975638703,0.0176496057587877));
#16222=CARTESIAN_POINT('',(-0.037761924286446,0.012028553013407,0.0180710725252609));
#16223=CARTESIAN_POINT('',(-0.0378872824673064,0.0118705612476647,0.0184049580447914));
#16224=CARTESIAN_POINT('',(-0.0379945248052401,0.0116137510202535,0.0187631780484681));
#16225=CARTESIAN_POINT('',(-0.0380645656555082,0.0112103498256101,0.0191337210208826));
#16226=CARTESIAN_POINT('',(-0.0380387434788214,0.0105616359467533,0.0194571705170615));
#16227=CARTESIAN_POINT('',(-0.0378458600825369,0.00984779301411321,0.0194914490882087));
#16228=CARTESIAN_POINT('',(-0.0376442920894866,0.00936086686795073,0.0193855797151924));
#16229=CARTESIAN_POINT('',(-0.0373865925798895,0.00887009516448303,0.0191803803526782));
#16230=CARTESIAN_POINT('',(-0.0371879791841231,0.00859580643238259,0.0189706556630093));
#16231=CARTESIAN_POINT('',(-0.0370209006250624,0.00841429288357993,0.0187724147329261));
#16232=CARTESIAN_POINT('',(-0.037020900637956,0.0084142929028602,0.0187724147537266));
#16233=CARTESIAN_POINT('',(-0.0370209006250624,0.00841429288357992,0.0187724147329261));
#16234=CARTESIAN_POINT('',(-0.0369382714896786,0.00832452489015545,0.0186743741699733));
#16235=CARTESIAN_POINT('',(-0.0368384384344524,0.00822765633725887,0.0185507187651021));
#16236=CARTESIAN_POINT('',(-0.0367214014593838,0.00813804549689372,0.0183955082750017));
#16237=CARTESIAN_POINT('',(-0.0345,-0.01,0.017320508076));
#16238=CARTESIAN_POINT('',(-0.0367214013837088,-0.0118619546747634,0.0162455081743171));
#16239=CARTESIAN_POINT('',(-0.0367099515900164,-0.011853187999615,0.0162303238456961));
#16240=CARTESIAN_POINT('',(-0.0366706595162203,-0.0118230656539648,0.0161785319969529));
#16241=CARTESIAN_POINT('',(-0.0365817713827235,-0.0117478247895692,0.0160659297903309));
#16242=CARTESIAN_POINT('',(-0.0364479212753901,-0.0116231137323535,0.01590491838796));
#16243=CARTESIAN_POINT('',(-0.0363510262352104,-0.0115197514139159,0.0157983752810768));
#16244=CARTESIAN_POINT('',(-0.0362580220090889,-0.0114165097628226,0.015699301101133));
#16245=CARTESIAN_POINT('',(-0.0361233040286148,-0.0112500280267554,0.0155680135421333));
#16246=CARTESIAN_POINT('',(-0.0360272389493788,-0.0111204221455142,0.0154825495970883));
#16247=CARTESIAN_POINT('',(-0.0359036157284611,-0.0109384327149448,0.0153831379251861));
#16248=CARTESIAN_POINT('',(-0.0357760361120856,-0.0107334813091317,0.0152928197612594));
#16249=CARTESIAN_POINT('',(-0.0355845872602139,-0.0103740954991592,0.0151911279464576));
#16250=CARTESIAN_POINT('',(-0.0354400098076825,-0.0100353939449807,0.0151588580332771));
#16251=CARTESIAN_POINT('',(-0.0352974513270221,-0.00958273159223996,0.015196863697529));
#16252=CARTESIAN_POINT('',(-0.0352033477140545,-0.00907651521044848,0.0153447680800186));
#16253=CARTESIAN_POINT('',(-0.0352316825933093,-0.00855557847003619,0.0156889710191991));
#16254=CARTESIAN_POINT('',(-0.0353617642821804,-0.00822761344513396,0.0160791448880825));
#16255=CARTESIAN_POINT('',(-0.0355339588539356,-0.00801012318586718,0.016476505190529));
#16256=CARTESIAN_POINT('',(-0.0356900436884747,-0.00790567375104684,0.0167851632262147));
#16257=CARTESIAN_POINT('',(-0.0358977301136069,-0.00785023313742566,0.0171562408720358));
#16258=CARTESIAN_POINT('',(-0.0360269463746216,-0.00784805814372892,0.0173712503749636));
#16259=CARTESIAN_POINT('',(-0.0361556833111774,-0.0078628285360704,0.0175781112952451));
#16260=CARTESIAN_POINT('',(-0.0362517163787167,-0.00788664178329998,0.0177265531559201));
#16261=CARTESIAN_POINT('',(-0.0363379367050056,-0.00791668749715034,0.0178562799663085));
#16262=CARTESIAN_POINT('',(-0.0363829297000817,-0.00793596622153825,0.0179223922516189));
#16263=CARTESIAN_POINT('',(-0.0363829296981285,-0.00793596622218309,0.0179223922530286));
#16264=CARTESIAN_POINT('',(-0.0367214015132256,-0.0118619576141813,0.0162455065977611));
#16265=CARTESIAN_POINT('',(-0.0363829297000817,-0.00793596622153825,0.0179223922516189));
#16266=CARTESIAN_POINT('',(-0.0364957535948001,-0.00798408903520211,0.018087419206871));
#16267=CARTESIAN_POINT('',(-0.0366085774895185,-0.0080520952982146,0.0182466381820913));
#16268=CARTESIAN_POINT('',(-0.0367214013842369,-0.00813804543863112,0.018395508174088));
#16269=CARTESIAN_POINT('',(-0.036721401387368,-0.00813803958757096,0.0183955115202174));
#16270=CARTESIAN_POINT('',(-0.0367214014593838,-0.00813804549645275,0.0183955082742379));
#16271=CARTESIAN_POINT('',(-0.0368094504194815,-0.00820546129496087,0.0185122758337679));
#16272=CARTESIAN_POINT('',(-0.0369082049132582,-0.00829303830385063,0.0186381461090242));
#16273=CARTESIAN_POINT('',(-0.037072915671782,-0.00846997252972903,0.0188345415312814));
#16274=CARTESIAN_POINT('',(-0.0372054109935089,-0.00862944346656265,0.0189847045417791));
#16275=CARTESIAN_POINT('',(-0.0374076787331404,-0.00892022797846519,0.019192476829662));
#16276=CARTESIAN_POINT('',(-0.0375742361574633,-0.00921722733948676,0.0193348101900589));
#16277=CARTESIAN_POINT('',(-0.0377617180565947,-0.00963510103336886,0.0194525250642369));
#16278=CARTESIAN_POINT('',(-0.0378881050762795,-0.0100063292794282,0.0194828665958168));
#16279=CARTESIAN_POINT('',(-0.0379944159747534,-0.0104434483789157,0.0194386388515495));
#16280=CARTESIAN_POINT('',(-0.0380653168371592,-0.0109630121629511,0.0192780031230472));
#16281=CARTESIAN_POINT('',(-0.0380390849645502,-0.0114596611018754,0.0189393960949147));
#16282=CARTESIAN_POINT('',(-0.0379290139211953,-0.0117932013607519,0.0185312293304056));
#16283=CARTESIAN_POINT('',(-0.0377914077671703,-0.0119983526985195,0.0181451922270323));
#16284=CARTESIAN_POINT('',(-0.0376479878208797,-0.0121064908415727,0.0178074590376732));
#16285=CARTESIAN_POINT('',(-0.0374402992125289,-0.0121604334017888,0.0173824654992756));
#16286=CARTESIAN_POINT('',(-0.0372619157386173,-0.0121430293010699,0.0170606766185285));
#16287=CARTESIAN_POINT('',(-0.0371044376010756,-0.012090702944845,0.0168013531294328));
#16288=CARTESIAN_POINT('',(-0.0370209006250624,-0.0120502416069907,0.0166731987585513));
#16289=CARTESIAN_POINT('',(-0.037020900637956,-0.0120502416154678,0.0166731987850141));
#16290=CARTESIAN_POINT('',(-0.0370209006250624,-0.0120502416069907,0.0166731987585513));
#16291=CARTESIAN_POINT('',(-0.0369382714896785,-0.0120102199855764,0.016546437114325));
#16292=CARTESIAN_POINT('',(-0.0368384384344523,-0.0119515655400817,0.0164007187842568));
#16293=CARTESIAN_POINT('',(-0.0367214014593838,-0.0118619547328937,0.0162455082750017));
#16294=CARTESIAN_POINT('',(-0.0345,-0.02,0.));
#16295=CARTESIAN_POINT('',(-0.0367214013837088,-0.0200000001135268,-0.00215));
#16296=CARTESIAN_POINT('',(-0.0367099515894606,-0.0199824667607752,-0.00215000000092581));
#16297=CARTESIAN_POINT('',(-0.0366706595152771,-0.0199225525306318,-0.00214980920870223));
#16298=CARTESIAN_POINT('',(-0.0365817713819794,-0.0197874157272833,-0.00214094981195455));
#16299=CARTESIAN_POINT('',(-0.036447921275795,-0.0195856202356591,-0.00211345256966799));
#16300=CARTESIAN_POINT('',(-0.0363510262352866,-0.0194416700387721,-0.00207720972953836));
#16301=CARTESIAN_POINT('',(-0.0362580220091507,-0.0193042484564968,-0.00203733692692017));
#16302=CARTESIAN_POINT('',(-0.0361233040282915,-0.0191073092266076,-0.00195880329346809));
#16303=CARTESIAN_POINT('',(-0.0360272389495356,-0.0189684923391471,-0.0018892932806967));
#16304=CARTESIAN_POINT('',(-0.0359036157281572,-0.0187914045898843,-0.00178139164613739));
#16305=CARTESIAN_POINT('',(-0.0357760361122662,-0.0186107110632828,-0.0016490576045929));
#16306=CARTESIAN_POINT('',(-0.0355845872601076,-0.0183429504628644,-0.00138866627045801));
#16307=CARTESIAN_POINT('',(-0.0354400098077096,-0.0181456531213779,-0.00111147707701261));
#16308=CARTESIAN_POINT('',(-0.0352974513270199,-0.0179522358156644,-0.000700457148026627));
#16309=CARTESIAN_POINT('',(-0.0352033477140541,-0.0178272165773168,-0.000188108710314427));
#16310=CARTESIAN_POINT('',(-0.0352316825933212,-0.0178648366965096,0.000435137210326799));
#16311=CARTESIAN_POINT('',(-0.0353617642821596,-0.0180387546663218,0.000914250187784095));
#16312=CARTESIAN_POINT('',(-0.03553395885398,-0.0182741336531804,0.00130128242879666));
#16313=CARTESIAN_POINT('',(-0.035690043688318,-0.0184892146354674,0.00154606731033654));
#16314=CARTESIAN_POINT('',(-0.0358977301136526,-0.0187828569970073,0.00177961911332545));
#16315=CARTESIAN_POINT('',(-0.0360269463745707,-0.0189679731916343,0.00188900746451258));
#16316=CARTESIAN_POINT('',(-0.03615568331116,-0.0191545051998607,0.00197964638970481));
#16317=CARTESIAN_POINT('',(-0.0362517163788373,-0.0192949662460136,0.00203324444307036));
#16318=CARTESIAN_POINT('',(-0.0363379367050595,-0.0194223358161986,0.00207208749675905));
#16319=CARTESIAN_POINT('',(-0.0363829297000817,-0.0194892300968965,0.00208844777432515));
#16320=CARTESIAN_POINT('',(-0.0363829296981285,-0.0194892300988016,0.00208844777506104));
#16321=CARTESIAN_POINT('',(-0.0367214015132256,-0.0200000002179966,-0.00215000333373415));
#16322=CARTESIAN_POINT('',(-0.0363829297000817,-0.0194892300968965,0.00208844777432515));
#16323=CARTESIAN_POINT('',(-0.0364957535948001,-0.0196562090026207,0.00212928566385514));
#16324=CARTESIAN_POINT('',(-0.0366085774895185,-0.019828099772606,0.00215));
#16325=CARTESIAN_POINT('',(-0.0367214013842369,-0.02,0.00215));
#16326=CARTESIAN_POINT('',(-0.0367214014187913,-0.0200000000544145,0.00215000673958342));
#16327=CARTESIAN_POINT('',(-0.0367214014855027,-0.0200000001547961,0.00214999999999999));
#16328=CARTESIAN_POINT('',(-0.0368094489890548,-0.0201348294968441,0.00214999999029253));
#16329=CARTESIAN_POINT('',(-0.0369082050670065,-0.0202876273874728,0.00213709176971192));
#16330=CARTESIAN_POINT('',(-0.0370729159603206,-0.020546178196832,0.00208205843123112));
#16331=CARTESIAN_POINT('',(-0.0372054092685199,-0.0207559551904642,0.00201904010762059));
#16332=CARTESIAN_POINT('',(-0.0374076931255592,-0.0210813111222118,0.00187105308343718));
#16333=CARTESIAN_POINT('',(-0.0375741836336396,-0.0213529605587038,0.00168520277677421));
#16334=CARTESIAN_POINT('',(-0.0377619138459259,-0.0216642665456907,0.00138145860675146));
#16335=CARTESIAN_POINT('',(-0.0378873214687462,-0.0218745084926748,0.0010778688280807));
#16336=CARTESIAN_POINT('',(-0.0379943792862313,-0.0220560156885546,0.00067569085601466));
#16337=CARTESIAN_POINT('',(-0.0380653382957039,-0.0221767836959647,0.000144366751129057));
#16338=CARTESIAN_POINT('',(-0.0380390815274064,-0.0221318227466957,-0.000454597526155525));
#16339=CARTESIAN_POINT('',(-0.0379290145646173,-0.0219451171585747,-0.00094760900861487));
#16340=CARTESIAN_POINT('',(-0.0377914075906246,-0.0217133734686235,-0.00131827900098319));
#16341=CARTESIAN_POINT('',(-0.0376479878638091,-0.0214749573987788,-0.0015807999458275));
#16342=CARTESIAN_POINT('',(-0.037440299198058,-0.0211338733786737,-0.00184001127321334));
#16343=CARTESIAN_POINT('',(-0.0372619157406907,-0.0208464940115701,-0.00198583361015462));
#16344=CARTESIAN_POINT('',(-0.0371044376005431,-0.020595750099457,-0.00207017933556629));
#16345=CARTESIAN_POINT('',(-0.0370209006250623,-0.0204645344905706,-0.0020992159743748));
#16346=CARTESIAN_POINT('',(-0.037020900637956,-0.020464534518328,-0.00209921596804585));
#16347=CARTESIAN_POINT('',(-0.0370209006250623,-0.0204645344905706,-0.0020992159743748));
#16348=CARTESIAN_POINT('',(-0.0369382714896785,-0.0203347448757318,-0.00212793705564823));
#16349=CARTESIAN_POINT('',(-0.0368384384344523,-0.0201792218773405,-0.00214999998084516));
#16350=CARTESIAN_POINT('',(-0.0367214014593838,-0.0200000002297874,-0.00214999999999999));
#16351=CARTESIAN_POINT('',(-0.0345,-0.01,-0.017320508076));
#16352=CARTESIAN_POINT('',(-0.0370209006250624,-0.00841429288357993,-0.0187724147329261));
#16353=CARTESIAN_POINT('',(-0.0369382714896786,-0.00832452489015546,-0.0186743741699733));
#16354=CARTESIAN_POINT('',(-0.0368384384344524,-0.00822765633725888,-0.0185507187651021));
#16355=CARTESIAN_POINT('',(-0.0367214014593838,-0.00813804549689372,-0.0183955082750017));
#16356=CARTESIAN_POINT('',(-0.0367214015196458,-0.00813804260431159,-0.0183955099312896));
#16357=CARTESIAN_POINT('',(-0.037020900637956,-0.0084142929028602,-0.0187724147537266));
#16358=CARTESIAN_POINT('',(-0.0367214013837088,-0.00813804543876341,-0.0183955081743171));
#16359=CARTESIAN_POINT('',(-0.0367099515902943,-0.00812927876222418,-0.0183803238469904));
#16360=CARTESIAN_POINT('',(-0.0366706595167001,-0.00809948687848419,-0.0183283412063308));
#16361=CARTESIAN_POINT('',(-0.0365817713830814,-0.00803959093902229,-0.01820687960295));
#16362=CARTESIAN_POINT('',(-0.0364479212752632,-0.00796250650282354,-0.0180183709572473));
#16363=CARTESIAN_POINT('',(-0.0363510262345629,-0.00792191862265392,-0.0178755850107191));
#16364=CARTESIAN_POINT('',(-0.0362580220107654,-0.00788773870098001,-0.0177366380263864));
#16365=CARTESIAN_POINT('',(-0.0361233040225563,-0.00785728117283103,-0.0175268168421644));
#16366=CARTESIAN_POINT('',(-0.0360272389715468,-0.00784807029588221,-0.0173718428532673));
#16367=CARTESIAN_POINT('',(-0.0359036156458474,-0.00785297149296298,-0.017164529662831));
#16368=CARTESIAN_POINT('',(-0.0357760365507627,-0.00787723178427133,-0.0169418768814245));
#16369=CARTESIAN_POINT('',(-0.0355845837251886,-0.00796883860250597,-0.0165797981192282));
#16370=CARTESIAN_POINT('',(-0.0354400227144834,-0.00811031891300495,-0.0162703208634176));
#16371=CARTESIAN_POINT('',(-0.035297403234844,-0.00836928163819279,-0.0158973739307318));
#16372=CARTESIAN_POINT('',(-0.0352036030273427,-0.00875188303428271,-0.0155325949701537));
#16373=CARTESIAN_POINT('',(-0.0352300877690043,-0.00930187689549947,-0.0152555942094222));
#16374=CARTESIAN_POINT('',(-0.0353624250665134,-0.00981312376305411,-0.0151648195632774));
#16375=CARTESIAN_POINT('',(-0.0355323875544582,-0.0102612841707686,-0.0151742083556311));
#16376=CARTESIAN_POINT('',(-0.0356952788199552,-0.0105915687258194,-0.0152431274376651));
#16377=CARTESIAN_POINT('',(-0.0359199076858085,-0.0109730735621656,-0.015389020528737));
#16378=CARTESIAN_POINT('',(-0.0361452214386918,-0.011283331940451,-0.0155847980942524));
#16379=CARTESIAN_POINT('',(-0.036292938920463,-0.011458027693942,-0.0157344351657852));
#16380=CARTESIAN_POINT('',(-0.0363829297000817,-0.0115532638753583,-0.0158339444772937));
#16381=CARTESIAN_POINT('',(-0.0363829296981285,-0.0115532638766184,-0.0158339444786343));
#16382=CARTESIAN_POINT('',(-0.0363829297000817,-0.0115532638753583,-0.0158339444772937));
#16383=CARTESIAN_POINT('',(-0.0364957535948001,-0.0116721200040918,-0.0159581335340468));
#16384=CARTESIAN_POINT('',(-0.0366085774895185,-0.0117760045498996,-0.0160966381730355));
#16385=CARTESIAN_POINT('',(-0.0367214013842369,-0.0118619546746311,-0.016245508174088));
#16386=CARTESIAN_POINT('',(-0.0367214014146637,-0.0118619604972779,-0.0162455047804234));
#16387=CARTESIAN_POINT('',(-0.0367214014593838,-0.0118619547324527,-0.016245508274238));
#16388=CARTESIAN_POINT('',(-0.0368094504192829,-0.0119293705059448,-0.0163622758478597));
#16389=CARTESIAN_POINT('',(-0.0369082047152049,-0.0119945891801026,-0.0165010543225801));
#16390=CARTESIAN_POINT('',(-0.0370729160019372,-0.0120762046321228,-0.0167524831086091));
#16391=CARTESIAN_POINT('',(-0.0372054092111889,-0.012126517585255,-0.0169656643348472));
#16392=CARTESIAN_POINT('',(-0.0374076931232449,-0.0121610350729264,-0.0173214244251849));
#16393=CARTESIAN_POINT('',(-0.0375741836148091,-0.0121359086968873,-0.0176496048646528));
#16394=CARTESIAN_POINT('',(-0.0377619138370843,-0.0120285115303349,-0.0180710758569835));
#16395=CARTESIAN_POINT('',(-0.0378873214603961,-0.0118707160469429,-0.0184049456120169));
#16396=CARTESIAN_POINT('',(-0.0379943792822431,-0.0116131733062125,-0.0187632244478438));
#16397=CARTESIAN_POINT('',(-0.0380653382950396,-0.0112134171394556,-0.0191334746681379));
#16398=CARTESIAN_POINT('',(-0.0380390815294286,-0.0106722183817588,-0.0193940194895447));
#16399=CARTESIAN_POINT('',(-0.0379290145681879,-0.0101519051183761,-0.0194788334521171));
#16400=CARTESIAN_POINT('',(-0.0377914075938042,-0.00971502363865889,-0.0194634725276762));
#16401=CARTESIAN_POINT('',(-0.0376479878673517,-0.00936846579559278,-0.0193882586280947));
#16402=CARTESIAN_POINT('',(-0.0374402992000195,-0.00897344018668948,-0.0192224768650296));
#16403=CARTESIAN_POINT('',(-0.0372619157421827,-0.0087034646538467,-0.0190465102007785));
#16404=CARTESIAN_POINT('',(-0.0371044376010715,-0.0085050471554441,-0.0188715324648092));
#16405=CARTESIAN_POINT('',(-0.0370209006250624,-0.00841429288357993,-0.0187724147329261));
#16406=CARTESIAN_POINT('',(-0.087860759494,-0.013728578874,0.019318802295));
#16407=CARTESIAN_POINT('',(-0.0385114728765227,-0.0140270889248519,0.0192889401143525));
#16408=CARTESIAN_POINT('',(-0.038573289075003,-0.0140394345481,0.0194123501448213));
#16409=CARTESIAN_POINT('',(-0.0386752804813098,-0.0139811072101053,0.0195073825579457));
#16410=CARTESIAN_POINT('',(-0.0387712812922,-0.0139023583533399,0.0195633440960825));
#16411=CARTESIAN_POINT('',(-0.0387712814781634,-0.0139023583534943,0.0195633440959764));
#16412=CARTESIAN_POINT('',(-0.0441999997501262,-0.01390235835348,0.019563344096154));
#16413=CARTESIAN_POINT('',(-0.0423904270131806,-0.01390235835348,0.019563344096154));
#16414=CARTESIAN_POINT('',(-0.0405808542762351,-0.01390235835348,0.019563344096154));
#16415=CARTESIAN_POINT('',(-0.0387712815392895,-0.01390235835348,0.019563344096154));
#16416=CARTESIAN_POINT('',(-0.087860759494,-0.009866284121,0.02154869921));
#16417=CARTESIAN_POINT('',(-0.04419999975,-0.00999117379127614,0.0218214675554262));
#16418=CARTESIAN_POINT('',(-0.0423904270660306,-0.00999117379127614,0.0218214675554262));
#16419=CARTESIAN_POINT('',(-0.0405808543820613,-0.00999117379127614,0.0218214675554262));
#16420=CARTESIAN_POINT('',(-0.038771281698092,-0.00999117379127614,0.0218214675554262));
#16421=CARTESIAN_POINT('',(-0.038771281698092,-0.0099911738207244,0.0218214675419355));
#16422=CARTESIAN_POINT('',(-0.0387712812921071,-0.00999117379334386,0.0218214675543855));
#16423=CARTESIAN_POINT('',(-0.0386753744229194,-0.00990342107731365,0.0218616459994942));
#16424=CARTESIAN_POINT('',(-0.0385732282122488,-0.00979177178844656,0.0218646104089203));
#16425=CARTESIAN_POINT('',(-0.0385114731132445,-0.00969116807386408,0.0217922856834247));
#16426=CARTESIAN_POINT('',(-0.087860759494,0.,0.));
#16427=CARTESIAN_POINT('',(-0.038771281292,-0.00999117382072726,0.0218214675419417));
#16428=CARTESIAN_POINT('',(-0.038771281292,-0.0113619672026171,0.0211938362919151));
#16429=CARTESIAN_POINT('',(-0.038771281292,-0.0126734170568365,0.0204366703644534));
#16430=CARTESIAN_POINT('',(-0.038771281292,-0.0139023583534153,0.0195633440958652));
#16431=CARTESIAN_POINT('',(-0.087860759494,0.009866284121,0.02154869921));
#16432=CARTESIAN_POINT('',(-0.0385114717026308,0.00969116577615237,0.0217922840320089));
#16433=CARTESIAN_POINT('',(-0.0385732483128315,0.00979180548548719,0.0218646360742229));
#16434=CARTESIAN_POINT('',(-0.0386753409989158,0.00990339049508929,0.0218616600018668));
#16435=CARTESIAN_POINT('',(-0.0387712812921071,0.00999117379334386,0.0218214675543855));
#16436=CARTESIAN_POINT('',(-0.0387712813225499,0.00999117382638656,0.0218214675391701));
#16437=CARTESIAN_POINT('',(-0.038771281542,0.0099911737873573,0.0218214675572204));
#16438=CARTESIAN_POINT('',(-0.040580854278,0.0099911737873573,0.0218214675572204));
#16439=CARTESIAN_POINT('',(-0.042390427014,0.0099911737873573,0.0218214675572204));
#16440=CARTESIAN_POINT('',(-0.04419999975,0.0099911737873573,0.0218214675572204));
#16441=CARTESIAN_POINT('',(-0.087860759494,0.013728578874,0.019318802295));
#16442=CARTESIAN_POINT('',(-0.03851147287724,0.0140270889244258,0.0192889401149925));
#16443=CARTESIAN_POINT('',(-0.038573288943412,0.0140394345209634,0.0194123498809255));
#16444=CARTESIAN_POINT('',(-0.0386752806869572,0.0139811070414031,0.0195073826778311));
#16445=CARTESIAN_POINT('',(-0.0387712812922,0.0139023583533399,0.0195633440960825));
#16446=CARTESIAN_POINT('',(-0.0387712813306431,0.0139023583200914,0.0195633441197136));
#16447=CARTESIAN_POINT('',(-0.0387712815392895,0.0139023583534361,0.0195633440961853));
#16448=CARTESIAN_POINT('',(-0.0405808542762351,0.0139023583534361,0.0195633440961853));
#16449=CARTESIAN_POINT('',(-0.0423904270131806,0.0139023583534361,0.0195633440961853));
#16450=CARTESIAN_POINT('',(-0.0441999997501262,0.0139023583534361,0.0195633440961853));
#16451=CARTESIAN_POINT('',(-0.087860759494,0.,0.));
#16452=CARTESIAN_POINT('',(-0.038771281292,0.0139023583499953,0.0195633440982956));
#16453=CARTESIAN_POINT('',(-0.038771281292,0.0126734170460618,0.0204366703717869));
#16454=CARTESIAN_POINT('',(-0.038771281292,0.0113619671835387,0.0211938363027715));
#16455=CARTESIAN_POINT('',(-0.038771281292,0.00999117379281267,0.0218214675547227));
#16456=CARTESIAN_POINT('',(-0.0442,0.0235948629949949,0.002229896915));
#16457=CARTESIAN_POINT('',(-0.0441999999970615,0.023893532146402,0.00225812346420597));
#16458=CARTESIAN_POINT('',(-0.0441999999970615,0.0238821025668367,0.0023790614791501));
#16459=CARTESIAN_POINT('',(-0.0441999999970615,0.0237898463900922,0.00248823412576593));
#16460=CARTESIAN_POINT('',(-0.0441999999970615,0.0236725087091264,0.00251967466286776));
#16461=CARTESIAN_POINT('',(-0.087860759494,0.023594862995,-0.002229896915));
#16462=CARTESIAN_POINT('',(-0.0387712815392895,0.0238935321468372,-0.00225812345819673));
#16463=CARTESIAN_POINT('',(-0.0405808542762351,0.0238935321468372,-0.00225812345819673));
#16464=CARTESIAN_POINT('',(-0.0423904270131806,0.0238935321468372,-0.00225812345819673));
#16465=CARTESIAN_POINT('',(-0.0441999997501262,0.0238935321468372,-0.00225812345819673));
#16466=CARTESIAN_POINT('',(-0.0387712813230477,0.0238935321497167,-0.00225812342724101));
#16467=CARTESIAN_POINT('',(-0.0385114731151673,0.0237182570486275,-0.00250334509570224));
#16468=CARTESIAN_POINT('',(-0.0385732893238704,0.0238313057094952,-0.00245233165510885));
#16469=CARTESIAN_POINT('',(-0.0386752804420734,0.0238844424877642,-0.00235430245929402));
#16470=CARTESIAN_POINT('',(-0.0387712812922245,0.0238935321467271,-0.00225812345823865));
#16471=CARTESIAN_POINT('',(-0.087860759494,0.,0.));
#16472=CARTESIAN_POINT('',(-0.038771281542,0.0238935321456456,0.00225812346983103));
#16473=CARTESIAN_POINT('',(-0.040580854278,0.0238935321456456,0.00225812346983103));
#16474=CARTESIAN_POINT('',(-0.042390427014,0.0238935321456456,0.00225812346983103));
#16475=CARTESIAN_POINT('',(-0.04419999975,0.0238935321456456,0.00225812346983103));
#16476=CARTESIAN_POINT('',(-0.0387712813158654,0.0238935321486615,0.0022581234372457));
#16477=CARTESIAN_POINT('',(-0.038771281292,0.,0.));
#16478=CARTESIAN_POINT('',(-0.087860759494,0.013728578874,-0.019318802295));
#16479=CARTESIAN_POINT('',(-0.0385114728779744,0.0140270889245724,-0.0192889401164586));
#16480=CARTESIAN_POINT('',(-0.0385732890765705,0.0140394345468466,-0.0194123501457808));
#16481=CARTESIAN_POINT('',(-0.0386752804819875,0.013981107209601,-0.0195073825583042));
#16482=CARTESIAN_POINT('',(-0.0387712812922,0.0139023583533399,-0.0195633440960825));
#16483=CARTESIAN_POINT('',(-0.0387712814781634,0.013902358347653,-0.0195633441001275));
#16484=CARTESIAN_POINT('',(-0.0441999997501262,0.0139023583533358,-0.0195633440962565));
#16485=CARTESIAN_POINT('',(-0.0423904270131806,0.0139023583533358,-0.0195633440962565));
#16486=CARTESIAN_POINT('',(-0.0405808542762351,0.0139023583533358,-0.0195633440962565));
#16487=CARTESIAN_POINT('',(-0.0387712815392895,0.0139023583533358,-0.0195633440962565));
#16488=CARTESIAN_POINT('',(-0.087860759494,0.009866284121,-0.02154869921));
#16489=CARTESIAN_POINT('',(-0.0385114728779643,0.00969116769057448,-0.0217922854078746));
#16490=CARTESIAN_POINT('',(-0.0385732889440606,0.00979187088396713,-0.0218646818897494));
#16491=CARTESIAN_POINT('',(-0.0386752807584405,0.00990333537634139,-0.0218616852385245));
#16492=CARTESIAN_POINT('',(-0.0387712812921071,0.00999117379334244,-0.0218214675543824));
#16493=CARTESIAN_POINT('',(-0.0387712813312419,0.00999117383538471,-0.0218214675352231));
#16494=CARTESIAN_POINT('',(-0.0387712815392895,0.00999117379350284,-0.0218214675543916));
#16495=CARTESIAN_POINT('',(-0.0405808542762351,0.00999117379350284,-0.0218214675543916));
#16496=CARTESIAN_POINT('',(-0.0423904270131806,0.00999117379350284,-0.0218214675543916));
#16497=CARTESIAN_POINT('',(-0.0441999997501262,0.00999117379350284,-0.0218214675543916));
#16498=CARTESIAN_POINT('',(-0.087860759494,0.,0.));
#16499=CARTESIAN_POINT('',(-0.038771281292,0.00999117380568283,-0.0218214675488299));
#16500=CARTESIAN_POINT('',(-0.038771281292,0.0113619671887648,-0.0211938362994007));
#16501=CARTESIAN_POINT('',(-0.038771281292,0.0126734170441997,-0.0204366703723515));
#16502=CARTESIAN_POINT('',(-0.038771281292,0.0139023583419703,-0.0195633441039984));
#16503=CARTESIAN_POINT('',(-0.087860759494,-0.009866284121,-0.02154869921));
#16504=CARTESIAN_POINT('',(-0.0385114728775843,-0.00969116768995542,-0.0217922854074296));
#16505=CARTESIAN_POINT('',(-0.0385732890761236,-0.00979187109936457,-0.0218646820449889));
#16506=CARTESIAN_POINT('',(-0.0386752805524257,-0.00990333518783425,-0.0218616853248344));
#16507=CARTESIAN_POINT('',(-0.0387712812921071,-0.00999117379334244,-0.0218214675543824));
#16508=CARTESIAN_POINT('',(-0.0387712814781634,-0.00999117379760892,-0.0218214675525191));
#16509=CARTESIAN_POINT('',(-0.0441999997501262,-0.00999117379345386,-0.021821467554414));
#16510=CARTESIAN_POINT('',(-0.0423904270131806,-0.00999117379345386,-0.021821467554414));
#16511=CARTESIAN_POINT('',(-0.0405808542762351,-0.00999117379345386,-0.021821467554414));
#16512=CARTESIAN_POINT('',(-0.0387712815392895,-0.00999117379345386,-0.021821467554414));
#16513=CARTESIAN_POINT('',(-0.087860759494,-0.013728578874,-0.019318802295));
#16514=CARTESIAN_POINT('',(-0.0385114728754421,-0.014027088925738,-0.019288940113728));
#16515=CARTESIAN_POINT('',(-0.03857328894209,-0.014039434522914,-0.0194123498813593));
#16516=CARTESIAN_POINT('',(-0.0386752806859938,-0.0139811070422414,-0.0195073826772354));
#16517=CARTESIAN_POINT('',(-0.0387712812922,-0.0139023583533399,-0.0195633440960825));
#16518=CARTESIAN_POINT('',(-0.0387712813300123,-0.0139023583246212,-0.0195633441164946));
#16519=CARTESIAN_POINT('',(-0.0387712815392895,-0.0139023583535364,-0.019563344096114));
#16520=CARTESIAN_POINT('',(-0.0405808542762351,-0.0139023583535364,-0.019563344096114));
#16521=CARTESIAN_POINT('',(-0.0423904270131806,-0.0139023583535364,-0.019563344096114));
#16522=CARTESIAN_POINT('',(-0.0441999997501262,-0.0139023583535364,-0.019563344096114));
#16523=CARTESIAN_POINT('',(-0.087860759494,0.,0.));
#16524=CARTESIAN_POINT('',(-0.038771281292,-0.0139023583580203,-0.0195633440925927));
#16525=CARTESIAN_POINT('',(-0.038771281292,-0.0126734170544451,-0.0204366703665882));
#16526=CARTESIAN_POINT('',(-0.038771281292,-0.0113619671922325,-0.0211938362981107));
#16527=CARTESIAN_POINT('',(-0.038771281292,-0.00999117380176398,-0.0218214675506242));
#16528=CARTESIAN_POINT('',(-0.087860759494,-0.023594862995,-0.002229896915));
#16529=CARTESIAN_POINT('',(-0.0385114728774445,-0.0237182566135284,-0.00250334529184601));
#16530=CARTESIAN_POINT('',(-0.0385732890757216,-0.0238313056460365,-0.0024523319000197));
#16531=CARTESIAN_POINT('',(-0.0386752803220459,-0.0238844424764206,-0.00235430257962145));
#16532=CARTESIAN_POINT('',(-0.0387712812922245,-0.0238935321467551,-0.00225812345824131));
#16533=CARTESIAN_POINT('',(-0.0387712814781634,-0.0238935321469843,-0.00225812345615336));
#16534=CARTESIAN_POINT('',(-0.0441999965249051,-0.0238935321468321,-0.00225812345825037));
#16535=CARTESIAN_POINT('',(-0.0423904248630333,-0.0238935321468321,-0.00225812345825037));
#16536=CARTESIAN_POINT('',(-0.0405808532011614,-0.0238935321468321,-0.00225812345825037));
#16537=CARTESIAN_POINT('',(-0.0387712815392895,-0.0238935321468321,-0.00225812345825037));
#16538=CARTESIAN_POINT('',(-0.087860759494,-0.023594862995,0.002229896915));
#16539=CARTESIAN_POINT('',(-0.0385114728763641,-0.0237182566134299,0.0025033452929254));
#16540=CARTESIAN_POINT('',(-0.0385732889426975,-0.023831305405075,0.00245233201003066));
#16541=CARTESIAN_POINT('',(-0.038675280526865,-0.0238844424958164,0.00235430237439214));
#16542=CARTESIAN_POINT('',(-0.0387712812922245,-0.0238935321467551,0.00225812345824131));
#16543=CARTESIAN_POINT('',(-0.0387712813303033,-0.02389353215034,0.00225812342064574));
#16544=CARTESIAN_POINT('',(-0.0387712815392895,-0.0238935321468256,0.00225812345831925));
#16545=CARTESIAN_POINT('',(-0.0405808531921476,-0.0238935321468256,0.00225812345831925));
#16546=CARTESIAN_POINT('',(-0.0423904248450057,-0.0238935321468256,0.00225812345831925));
#16547=CARTESIAN_POINT('',(-0.0441999964978638,-0.0238935321468256,0.00225812345831925));
#16548=CARTESIAN_POINT('',(-0.087860759494,0.,0.));
#16549=CARTESIAN_POINT('',(-0.038771281292,-0.0238935321466156,0.00225812345956669));
#16550=CARTESIAN_POINT('',(-0.038771281292,-0.0240353842336054,0.000757165933885015));
#16551=CARTESIAN_POINT('',(-0.038771281292,-0.02403538423378,-0.000757165928341963));
#16552=CARTESIAN_POINT('',(-0.038771281292,-0.0238935321471364,-0.00225812345405635));
#16553=CARTESIAN_POINT('',(-0.0363829297,0.007935966222,-0.017922392252));
#16554=CARTESIAN_POINT('',(-0.036137554584,0.007975350095,-0.01805745087));
#16555=CARTESIAN_POINT('',(-0.036123122079,0.007706601765,-0.018144438831));
#16556=CARTESIAN_POINT('',(-0.036296388628,0.00789888486,-0.017795229609));
#16557=CARTESIAN_POINT('',(-0.036059352191,0.00792917773300001,-0.017929626577));
#16558=CARTESIAN_POINT('',(-0.03603658062,0.007664471384,-0.017999478691));
#16559=CARTESIAN_POINT('',(-0.036211750879,0.007873865053,-0.017666078425));
#16560=CARTESIAN_POINT('',(-0.03598108599,0.007894696976,-0.017796520282));
#16561=CARTESIAN_POINT('',(-0.035951943258,0.00763618434,-0.017852211978));
#16562=CARTESIAN_POINT('',(-0.036046427611,0.007847575992,-0.017403812149));
#16563=CARTESIAN_POINT('',(-0.03582764111,0.00785209075899999,-0.01752422126));
#16564=CARTESIAN_POINT('',(-0.03578661999,0.007606880233,-0.017553069188));
#16565=CARTESIAN_POINT('',(-0.035965731891,0.007846286179,-0.017270695297));
#16566=CARTESIAN_POINT('',(-0.035752240428,0.00784321052600001,-0.017384956612));
#16567=CARTESIAN_POINT('',(-0.03570592427,0.00760583974,-0.017401191901));
#16568=CARTESIAN_POINT('',(-0.035867783855,0.007860916809,-0.017101471238));
#16569=CARTESIAN_POINT('',(-0.035659677357,0.00785025534,-0.017205405462));
#16570=CARTESIAN_POINT('',(-0.035607976234,0.007623195358,-0.017208053208));
#16571=CARTESIAN_POINT('',(-0.03584830488,0.007864675489,-0.017067415562));
#16572=CARTESIAN_POINT('',(-0.035641412325,0.007852547538,-0.017169542439));
#16573=CARTESIAN_POINT('',(-0.035588497259,0.007627622941,-0.017169181517));
#16574=CARTESIAN_POINT('',(-0.035810061793,0.007873792339,-0.016999715979));
#16575=CARTESIAN_POINT('',(-0.035605524332,0.00785891862899999,-0.017098165957));
#16576=CARTESIAN_POINT('',(-0.035550254172,0.007638313039,-0.017091901304));
#16577=CARTESIAN_POINT('',(-0.035791254693,0.00787915358,-0.016965999395));
#16578=CARTESIAN_POINT('',(-0.035587855191,0.00786298741,-0.01706256955));
#16579=CARTESIAN_POINT('',(-0.035531447072,0.007644579318,-0.017053409847));
#16580=CARTESIAN_POINT('',(-0.035735788251,0.007897644484,-0.016865244352));
#16581=CARTESIAN_POINT('',(-0.035535852231,0.007877830875,-0.016956380478));
#16582=CARTESIAN_POINT('',(-0.03547598063,0.007666140505,-0.016938375535));
#16583=CARTESIAN_POINT('',(-0.035700081089,0.007913175312,-0.016798599729));
#16584=CARTESIAN_POINT('',(-0.035502196601,0.007891267476,-0.016885756544));
#16585=CARTESIAN_POINT('',(-0.035440273468,0.007684190871,-0.016862271769));
#16586=CARTESIAN_POINT('',(-0.035596955729,0.007969579454,-0.016600233953));
#16587=CARTESIAN_POINT('',(-0.035405412743,0.007942282341,-0.016676313757));
#16588=CARTESIAN_POINT('',(-0.035337148108,0.007749601706,-0.016635705408));
#16589=CARTESIAN_POINT('',(-0.035533471872,0.008020130655,-0.016470062373));
#16590=CARTESIAN_POINT('',(-0.03534514464,0.007990615333,-0.016537412932));
#16591=CARTESIAN_POINT('',(-0.035273664252,0.00780806873,-0.016486967212));
#16592=CARTESIAN_POINT('',(-0.035462076716,0.008101852446,-0.016310148785));
#16593=CARTESIAN_POINT('',(-0.0352770564989999,0.008072198153,-0.016365801681));
#16594=CARTESIAN_POINT('',(-0.035202269094,0.007902417857,-0.016304149447));
#16595=CARTESIAN_POINT('',(-0.035448157312,0.008119195502,-0.016278204166));
#16596=CARTESIAN_POINT('',(-0.035263851039,0.008089510152,-0.016331706315));
#16597=CARTESIAN_POINT('',(-0.035188349691,0.007922433981,-0.016267624501));
#16598=CARTESIAN_POINT('',(-0.035421421576,0.008155528492,-0.01621518104));
#16599=CARTESIAN_POINT('',(-0.035238481118,0.008125981757,-0.0162644302));
#16600=CARTESIAN_POINT('',(-0.035161613954,0.007964353608,-0.016195554481));
#16601=CARTESIAN_POINT('',(-0.035408615027,0.008174492909,-0.016184132248));
#16602=CARTESIAN_POINT('',(-0.035226318844,0.008145113188,-0.016231268977));
#16603=CARTESIAN_POINT('',(-0.035148807406,0.007986227718,-0.01616004343));
#16604=CARTESIAN_POINT('',(-0.035371903227,0.008233790533,-0.016092375852));
#16605=CARTESIAN_POINT('',(-0.035191509303,0.008205098964,-0.016133439925));
#16606=CARTESIAN_POINT('',(-0.035112095605,0.008054604749,-0.016055083828));
#16607=CARTESIAN_POINT('',(-0.035349701075,0.00827652121,-0.01603305419));
#16608=CARTESIAN_POINT('',(-0.035170375015,0.00824874590400001,-0.016070010593));
#16609=CARTESIAN_POINT('',(-0.035089893455,0.008103854486,-0.015987204245));
#16610=CARTESIAN_POINT('',(-0.035310076825,0.008368595603,-0.015918211266));
#16611=CARTESIAN_POINT('',(-0.035132682741,0.008343387593,-0.015947352599));
#16612=CARTESIAN_POINT('',(-0.035050269204,0.008209928279,-0.015855746634));
#16613=CARTESIAN_POINT('',(-0.035292653375,0.008417937511,-0.015862688976));
#16614=CARTESIAN_POINT('',(-0.035116074086,0.00839440358600001,-0.015888019139));
#16615=CARTESIAN_POINT('',(-0.035032845755,0.008266750265,-0.015792167434));
#16616=CARTESIAN_POINT('',(-0.035270404132,0.008497251596,-0.015782437272));
#16617=CARTESIAN_POINT('',(-0.035094864144,0.008476841102,-0.015802332322));
#16618=CARTESIAN_POINT('',(-0.03501059651,0.00835805282,-0.015700230057));
#16619=CARTESIAN_POINT('',(-0.03526362249,0.008524662259,-0.015756120857));
#16620=CARTESIAN_POINT('',(-0.035088401673,0.008505365652,-0.015774270534));
#16621=CARTESIAN_POINT('',(-0.035003814869,0.008389601082,-0.015670074582));
#16622=CARTESIAN_POINT('',(-0.035251577427,0.008580564888,-0.015705227052));
#16623=CARTESIAN_POINT('',(-0.035076925826,0.008563640037,-0.01572005437));
#16624=CARTESIAN_POINT('',(-0.034991769806,0.008453930794,-0.015611741863));
#16625=CARTESIAN_POINT('',(-0.035246291308,0.008609118788,-0.015680578683));
#16626=CARTESIAN_POINT('',(-0.035071886429,0.00859346260300001,-0.015693811186));
#16627=CARTESIAN_POINT('',(-0.034986483687,0.008486783572,-0.015583483346));
#16628=CARTESIAN_POINT('',(-0.035223521483,0.008754870702,-0.01556128769));
#16629=CARTESIAN_POINT('',(-0.035050225188,0.008745616554,-0.015567192245));
#16630=CARTESIAN_POINT('',(-0.034963713862,0.008654451161,-0.015446682695));
#16631=CARTESIAN_POINT('',(-0.035216913712,0.008880915106,-0.0154783625));
#16632=CARTESIAN_POINT('',(-0.035043883179,0.008878570113,-0.015479125626));
#16633=CARTESIAN_POINT('',(-0.034957106091,0.00879936203,-0.015351462313));
#16634=CARTESIAN_POINT('',(-0.035223876434,0.009050786794,-0.015391012352));
#16635=CARTESIAN_POINT('',(-0.035050518048,0.009057568695,-0.015387635792));
#16636=CARTESIAN_POINT('',(-0.034964068813,0.008994538787,-0.015250984281));
#16637=CARTESIAN_POINT('',(-0.03522604562,0.00908540579,-0.015374366785));
#16638=CARTESIAN_POINT('',(-0.035052587043,0.009094097267,-0.015370243184));
#16639=CARTESIAN_POINT('',(-0.034966237999,0.009034309077,-0.015231826369));
#16640=CARTESIAN_POINT('',(-0.035231850552,0.009154857947,-0.015343216139));
#16641=CARTESIAN_POINT('',(-0.035058120997,0.009167395622,-0.015337818228));
#16642=CARTESIAN_POINT('',(-0.034972042931,0.009114084127,-0.015195952232));
#16643=CARTESIAN_POINT('',(-0.0352354894,0.009189818174,-0.015328642479));
#16644=CARTESIAN_POINT('',(-0.035061591095,0.009204314377,-0.015322709066));
#16645=CARTESIAN_POINT('',(-0.034975681779,0.009154234899,-0.01517915715));
#16646=CARTESIAN_POINT('',(-0.035248550352,0.009295383715,-0.015287847634));
#16647=CARTESIAN_POINT('',(-0.035074046816,0.00931586337800001,-0.015280597597));
#16648=CARTESIAN_POINT('',(-0.034988742731,0.009275456669,-0.01513210841));
#16649=CARTESIAN_POINT('',(-0.035260111701,0.009366671914,-0.015264544541));
#16650=CARTESIAN_POINT('',(-0.035085080525,0.009391243379,-0.015256839807));
#16651=CARTESIAN_POINT('',(-0.03500030408,0.009357294881,-0.01510518209));
#16652=CARTESIAN_POINT('',(-0.035281577861,0.009474939166,-0.015235272178));
#16653=CARTESIAN_POINT('',(-0.035105505104,0.009505505488,-0.015227540121));
#16654=CARTESIAN_POINT('',(-0.03502177024,0.009481550391,-0.01507127367));
#16655=CARTESIAN_POINT('',(-0.035289421938,0.009511251248,-0.015226463836));
#16656=CARTESIAN_POINT('',(-0.035112977015,0.009543870113,-0.01521881712));
#16657=CARTESIAN_POINT('',(-0.035029614317,0.009523219169,-0.015061053398));
#16658=CARTESIAN_POINT('',(-0.035306476701,0.009584322003,-0.01521074306));
#16659=CARTESIAN_POINT('',(-0.035129211644,0.00962103848500001,-0.015203474112));
#16660=CARTESIAN_POINT('',(-0.03504666908,0.009607057743,-0.015042775596));
#16661=CARTESIAN_POINT('',(-0.035315718145,0.009621192412,-0.015203814));
#16662=CARTESIAN_POINT('',(-0.035138009535,0.00965997509200001,-0.015196840927));
#16663=CARTESIAN_POINT('',(-0.035055910524,0.0096493557,-0.015034698584));
#16664=CARTESIAN_POINT('',(-0.035345244257,0.009731576519,-0.015186028085));
#16665=CARTESIAN_POINT('',(-0.035166136457,0.00977663711299999,-0.015180221674));
#16666=CARTESIAN_POINT('',(-0.035085436637,0.009775971844,-0.01501389589));
#16667=CARTESIAN_POINT('',(-0.035367258146,0.009804686247,-0.01517816092));
#16668=CARTESIAN_POINT('',(-0.035187092355,0.009853788047,-0.015173570618));
#16669=CARTESIAN_POINT('',(-0.035107450524,0.009859809659,-0.015004586152));
#16670=CARTESIAN_POINT('',(-0.035415540032,0.009950034894,-0.01516985648));
#16671=CARTESIAN_POINT('',(-0.035232955499,0.010006887199,-0.015168405072));
#16672=CARTESIAN_POINT('',(-0.035155732411,0.01002644331,-0.014994457537));
#16673=CARTESIAN_POINT('',(-0.035441809443,0.010022273518,-0.015169421497));
#16674=CARTESIAN_POINT('',(-0.035257918294,0.010082919856,-0.015169944486));
#16675=CARTESIAN_POINT('',(-0.035182001822,0.0101092388,-0.014993641282));
#16676=CARTESIAN_POINT('',(-0.035498359317,0.010165935271,-0.01517571553));
#16677=CARTESIAN_POINT('',(-0.035311533473,0.010233771266,-0.015180838497));
#16678=CARTESIAN_POINT('',(-0.035238551696,0.01027385273,-0.015000197616));
#16679=CARTESIAN_POINT('',(-0.035528803299,0.010237694895,-0.015182511514));
#16680=CARTESIAN_POINT('',(-0.035340397738,0.010309011127,-0.01519034352));
#16681=CARTESIAN_POINT('',(-0.035268995678,0.010356056437,-0.015007645243));
#16682=CARTESIAN_POINT('',(-0.035624302868,0.010448231116,-0.015212973614));
#16683=CARTESIAN_POINT('',(-0.035431143853,0.010530150409,-0.015229867744));
#16684=CARTESIAN_POINT('',(-0.035364495247,0.010597173211,-0.015041521636));
#16685=CARTESIAN_POINT('',(-0.035693625065,0.010582922476,-0.015246481917));
#16686=CARTESIAN_POINT('',(-0.035496770299,0.010670383783,-0.015270793079));
#16687=CARTESIAN_POINT('',(-0.035433817443,0.010751346613,-0.015079216188));
#16688=CARTESIAN_POINT('',(-0.035804878296,0.010777396222,-0.015314797255));
#16689=CARTESIAN_POINT('',(-0.035600812464,0.010870193851,-0.015350654782));
#16690=CARTESIAN_POINT('',(-0.035545070675,0.010973839943,-0.015156427299));
#16691=CARTESIAN_POINT('',(-0.035843360668,0.010841212942,-0.01534073771));
#16692=CARTESIAN_POINT('',(-0.035636958249,0.01093587108,-0.015380883423));
#16693=CARTESIAN_POINT('',(-0.035583553047,0.011046831996,-0.015185790742));
#16694=CARTESIAN_POINT('',(-0.035921655233,0.010964716188,-0.015397891995));
#16695=CARTESIAN_POINT('',(-0.035710302083,0.011062419569,-0.015446810101));
#16696=CARTESIAN_POINT('',(-0.035661847612,0.011188055569,-0.01525056404));
#16697=CARTESIAN_POINT('',(-0.035961464931,0.011024436082,-0.015429078645));
#16698=CARTESIAN_POINT('',(-0.035747535996,0.011123315491,-0.015482566139));
#16699=CARTESIAN_POINT('',(-0.035701657309,0.011256325476,-0.015285942678));
#16700=CARTESIAN_POINT('',(-0.036082708725,0.011197835672,-0.015530092476));
#16701=CARTESIAN_POINT('',(-0.035861344783,0.01130037601,-0.015598213312));
#16702=CARTESIAN_POINT('',(-0.035822901104,0.011454498054,-0.015400624625));
#16703=CARTESIAN_POINT('',(-0.036165937985,0.011305805198,-0.015607312287));
#16704=CARTESIAN_POINT('',(-0.035938765603,0.011408558316,-0.015685491612));
#16705=CARTESIAN_POINT('',(-0.035906130364,0.011577821075,-0.015488403863));
#16706=CARTESIAN_POINT('',(-0.036272749616,0.011431478006,-0.015715991043));
#16707=CARTESIAN_POINT('',(-0.036036325391,0.011531489845,-0.015805195535));
#16708=CARTESIAN_POINT('',(-0.036012941995,0.011721279377,-0.015612059748));
#16709=CARTESIAN_POINT('',(-0.036294271622,0.011456162931,-0.015738362019));
#16710=CARTESIAN_POINT('',(-0.036056160144,0.011555785974,-0.015830037016));
#16711=CARTESIAN_POINT('',(-0.036034464001,0.011749453109,-0.015637518901));
#16712=CARTESIAN_POINT('',(-0.036337241164,0.011504198589,-0.015783958945));
#16713=CARTESIAN_POINT('',(-0.036095695252,0.011602868295,-0.015880530299));
#16714=CARTESIAN_POINT('',(-0.036077433543,0.011804268644,-0.015689420125));
#16715=CARTESIAN_POINT('',(-0.036358730845,0.011527600241,-0.015807226781));
#16716=CARTESIAN_POINT('',(-0.03611543566,0.011625696687,-0.015906237255));
#16717=CARTESIAN_POINT('',(-0.036098923223,0.011830968578,-0.015715909844));
#16718=CARTESIAN_POINT('',(-0.036423211553,0.011595992591,-0.015878412814));
#16719=CARTESIAN_POINT('',(-0.036174782484,0.011692352266,-0.015984962597));
#16720=CARTESIAN_POINT('',(-0.036163403931,0.011908986452,-0.015796966748));
#16721=CARTESIAN_POINT('',(-0.036466213928,0.011639174576,-0.015927710753));
#16722=CARTESIAN_POINT('',(-0.036214084658,0.011733813027,-0.016039055431));
#16723=CARTESIAN_POINT('',(-0.036206406307,0.011958226934,-0.015853118487));
#16724=CARTESIAN_POINT('',(-0.036595254777,0.011761619038,-0.016081028728));
#16725=CARTESIAN_POINT('',(-0.03633245937,0.011851005228,-0.016207593429));
#16726=CARTESIAN_POINT('',(-0.036335447156,0.012097793945,-0.016027801545));
#16727=CARTESIAN_POINT('',(-0.036681322249,0.01183384166,-0.01619042867));
#16728=CARTESIAN_POINT('',(-0.036410235723,0.011917375548,-0.016326105441));
#16729=CARTESIAN_POINT('',(-0.036421514628,0.012180036844,-0.016152509941));
#16730=CARTESIAN_POINT('',(-0.03678899075,0.011911891549,-0.016336502043));
#16731=CARTESIAN_POINT('',(-0.036505370032,0.01198586263,-0.016480211706));
#16732=CARTESIAN_POINT('',(-0.036529183129,0.012268805633,-0.016319094869));
#16733=CARTESIAN_POINT('',(-0.036810556304,0.011926900857,-0.016366226459));
#16734=CARTESIAN_POINT('',(-0.036524605066,0.011999026208,-0.016511861903));
#16735=CARTESIAN_POINT('',(-0.036550748683,0.012285869776,-0.016352996559));
#16736=CARTESIAN_POINT('',(-0.036853337272,0.011955422756,-0.016426124399));
#16737=CARTESIAN_POINT('',(-0.036562661331,0.012023724111,-0.016575442629));
#16738=CARTESIAN_POINT('',(-0.036593529651,0.012318283097,-0.016421318697));
#16739=CARTESIAN_POINT('',(-0.036874593816,0.011968966814,-0.016456352488));
#16740=CARTESIAN_POINT('',(-0.036581516731,0.012035273907,-0.016607435016));
#16741=CARTESIAN_POINT('',(-0.036614786195,0.012333668079,-0.016455801366));
#16742=CARTESIAN_POINT('',(-0.036937968442,0.012007462527,-0.016547866518));
#16743=CARTESIAN_POINT('',(-0.03663781018,0.012067727143,-0.016704386433));
#16744=CARTESIAN_POINT('',(-0.03667816082,0.012377374469,-0.016560205216));
#16745=CARTESIAN_POINT('',(-0.03697969206,0.01203028214,-0.016609980557));
#16746=CARTESIAN_POINT('',(-0.036674489896,0.012086090141,-0.016769529197));
#16747=CARTESIAN_POINT('',(-0.036719884461,0.012403252403,-0.016631080369));
#16748=CARTESIAN_POINT('',(-0.037020900622,0.012050241607,-0.016673198758));
#16749=CARTESIAN_POINT('',(-0.036710197303,0.012101269023,-0.016834819376));
#16750=CARTESIAN_POINT('',(-0.036761093001,0.012425852784,-0.016703226885));
#16751=CARTESIAN_POINT('',(-0.0370209006219633,0.0123363218309527,-0.0165828765281445));
#16752=CARTESIAN_POINT('',(-0.0363829297000878,0.00764796150808044,-0.0180063760900247));
#16753=CARTESIAN_POINT('',(-0.0370209006725265,0.0120502416314727,-0.016673198835513));
#16754=CARTESIAN_POINT('',(-0.0367101973471479,0.0121012690417669,-0.0168348194567234));
#16755=CARTESIAN_POINT('',(-0.0367610930515268,0.0124258528117109,-0.0167032269734606));
#16756=CARTESIAN_POINT('',(-0.037103317012847,0.0120901601826742,-0.0167996340374687));
#16757=CARTESIAN_POINT('',(-0.0367834353017993,0.0121324018021573,-0.0169687333890695));
#16758=CARTESIAN_POINT('',(-0.0368435097848469,0.0124710533801557,-0.0168475194030382));
#16759=CARTESIAN_POINT('',(-0.0371836845969985,0.012118723833302,-0.0169304571286969));
#16760=CARTESIAN_POINT('',(-0.036852619292111,0.0121502141620385,-0.0171032960490522));
#16761=CARTESIAN_POINT('',(-0.0369238769759985,0.0125032416596733,-0.016996863092627));
#16762=CARTESIAN_POINT('',(-0.037301116085,0.012142960991,-0.017133757444));
#16763=CARTESIAN_POINT('',(-0.03695137278,0.012158036728,-0.017307056189));
#16764=CARTESIAN_POINT('',(-0.037041308464,0.012530204072,-0.017229010285));
#16765=CARTESIAN_POINT('',(-0.037339424126,0.012147832408,-0.017202180744));
#16766=CARTESIAN_POINT('',(-0.036983551057,0.01215730462,-0.01737562732));
#16767=CARTESIAN_POINT('',(-0.037079616505,0.012535518531,-0.017307152903));
#16768=CARTESIAN_POINT('',(-0.037413681214,0.012151009491,-0.017339044018));
#16769=CARTESIAN_POINT('',(-0.037045412802,0.012149475489,-0.017511610772));
#16770=CARTESIAN_POINT('',(-0.037153873593,0.012538634267,-0.017463477304));
#16771=CARTESIAN_POINT('',(-0.037449744946,0.012149340492,-0.017407681576));
#16772=CARTESIAN_POINT('',(-0.037075133644,0.012142279398,-0.017579166281));
#16773=CARTESIAN_POINT('',(-0.037189937325,0.012536463788,-0.017541884702));
#16774=CARTESIAN_POINT('',(-0.037519742735,0.012139323808,-0.017545357834));
#16775=CARTESIAN_POINT('',(-0.037132298021,0.012121588311,-0.017713430993));
#16776=CARTESIAN_POINT('',(-0.037259935114,0.012524478835,-0.017699177365));
#16777=CARTESIAN_POINT('',(-0.037553677068,0.012130977326,-0.017614396504));
#16778=CARTESIAN_POINT('',(-0.037159681014,0.012107993462,-0.017780075124));
#16779=CARTESIAN_POINT('',(-0.037293869447,0.012514665743,-0.017778062592));
#16780=CARTESIAN_POINT('',(-0.037602938649,0.0121131804,-0.017718254592));
#16781=CARTESIAN_POINT('',(-0.037198872381,0.012082909484,-0.01787893623));
#16782=CARTESIAN_POINT('',(-0.037343131027,0.012493905947,-0.017896748231));
#16783=CARTESIAN_POINT('',(-0.037619085386,0.012106366928,-0.017752924047));
#16784=CARTESIAN_POINT('',(-0.037211691522,0.012073695505,-0.01791189675));
#16785=CARTESIAN_POINT('',(-0.037359277765,0.012485977458,-0.017936369838));
#16786=CARTESIAN_POINT('',(-0.037650817756,0.012090910276,-0.017822364053));
#16787=CARTESIAN_POINT('',(-0.037236742776,0.012053626329,-0.017977570801));
#16788=CARTESIAN_POINT('',(-0.037391010135,0.012468026175,-0.018015733672));
#16789=CARTESIAN_POINT('',(-0.037666411882,0.012082254089,-0.017857158743));
#16790=CARTESIAN_POINT('',(-0.037248972401,0.012042747188,-0.018010293639));
#16791=CARTESIAN_POINT('',(-0.037406604261,0.012457988408,-0.018055503508));
#16792=CARTESIAN_POINT('',(-0.037742059103,0.012034811789,-0.018029350412));
#16793=CARTESIAN_POINT('',(-0.037308672836,0.011984184277,-0.018173339907));
#16794=CARTESIAN_POINT('',(-0.037482251481,0.012403043831,-0.018252328917));
#16795=CARTESIAN_POINT('',(-0.037795953594,0.0119833468,-0.018163051804));
#16796=CARTESIAN_POINT('',(-0.0373492095610001,0.01192624568,-0.018295048154));
#16797=CARTESIAN_POINT('',(-0.037536145973,0.012343640815,-0.018405198115));
#16798=CARTESIAN_POINT('',(-0.037866774638,0.011884976998,-0.018357148242));
#16799=CARTESIAN_POINT('',(-0.037401307565,0.01182386073,-0.018467879798));
#16800=CARTESIAN_POINT('',(-0.037606967016,0.012230324528,-0.018627184794));
#16801=CARTESIAN_POINT('',(-0.037888699602,0.011848634259,-0.018420763928));
#16802=CARTESIAN_POINT('',(-0.037417279271,0.011786751401,-0.018524231365));
#16803=CARTESIAN_POINT('',(-0.037628891981,0.012188489579,-0.018699952716));
#16804=CARTESIAN_POINT('',(-0.037918925522,0.011788411713,-0.018514434973));
#16805=CARTESIAN_POINT('',(-0.037439020962,0.011726989924,-0.018606332456));
#16806=CARTESIAN_POINT('',(-0.037659117901,0.012119208257,-0.018807118231));
#16807=CARTESIAN_POINT('',(-0.037928582819,0.011767311068,-0.018545460028));
#16808=CARTESIAN_POINT('',(-0.037445936687,0.011706228285,-0.018633469683));
#16809=CARTESIAN_POINT('',(-0.037668775198,0.01209494007,-0.018842615969));
#16810=CARTESIAN_POINT('',(-0.037946745879,0.011723686791,-0.018606120592));
#16811=CARTESIAN_POINT('',(-0.037458875717,0.011663774496,-0.018686340803));
#16812=CARTESIAN_POINT('',(-0.037686938258,0.012044779429,-0.018912028045));
#16813=CARTESIAN_POINT('',(-0.03795527555,0.011701127516,-0.01863582313));
#16814=CARTESIAN_POINT('',(-0.037464908394,0.011642051742,-0.018712112891));
#16815=CARTESIAN_POINT('',(-0.037695467929,0.012018845928,-0.018946019049));
#16816=CARTESIAN_POINT('',(-0.037995201404,0.011584625415,-0.018781219738));
#16817=CARTESIAN_POINT('',(-0.037493219634,0.01153014651,-0.018838837483));
#16818=CARTESIAN_POINT('',(-0.037735393783,0.011884946284,-0.019112424772));
#16819=CARTESIAN_POINT('',(-0.03801852767,0.011479690222,-0.018887669477));
#16820=CARTESIAN_POINT('',(-0.037508976952,0.011433957386,-0.018929023907));
#16821=CARTESIAN_POINT('',(-0.037758720049,0.011764426365,-0.019234309834));
#16822=CARTESIAN_POINT('',(-0.038040144091,0.011303793235,-0.019031755487));
#16823=CARTESIAN_POINT('',(-0.037523624808,0.011276525335,-0.019052132642));
#16824=CARTESIAN_POINT('',(-0.03778033647,0.011562515578,-0.019399384648));
#16825=CARTESIAN_POINT('',(-0.038045091154,0.011241659818,-0.019077372673));
#16826=CARTESIAN_POINT('',(-0.0375269479359999,0.011221473817,-0.019091228452));
#16827=CARTESIAN_POINT('',(-0.037785283533,0.011491209999,-0.019451665162));
#16828=CARTESIAN_POINT('',(-0.038050108278,0.011114326029,-0.019160771595));
#16829=CARTESIAN_POINT('',(-0.037530327064,0.011109308985,-0.019163421876));
#16830=CARTESIAN_POINT('',(-0.037790300657,0.011345109716,-0.019547286114));
#16831=CARTESIAN_POINT('',(-0.038050243047,0.011048838426,-0.019198846514));
#16832=CARTESIAN_POINT('',(-0.037530417095,0.011052089911,-0.019196655463));
#16833=CARTESIAN_POINT('',(-0.037790435426,0.011269985121,-0.019590962239));
#16834=CARTESIAN_POINT('',(-0.038045857381,0.010914292279,-0.019267887587));
#16835=CARTESIAN_POINT('',(-0.037527464034,0.01093462983,-0.019257973428));
#16836=CARTESIAN_POINT('',(-0.03778604976,0.011115665703,-0.019670206775));
#16837=CARTESIAN_POINT('',(-0.038041336883,0.010845233676,-0.019298853626));
#16838=CARTESIAN_POINT('',(-0.037524429559,0.010874566119,-0.019285974336));
#16839=CARTESIAN_POINT('',(-0.037781529262,0.011036470818,-0.019705775052));
#16840=CARTESIAN_POINT('',(-0.038027559938,0.010703495215,-0.019353576094));
#16841=CARTESIAN_POINT('',(-0.037515080889,0.010750844555,-0.019336843363));
#16842=CARTESIAN_POINT('',(-0.037767752317,0.010873951929,-0.019768689912));
#16843=CARTESIAN_POINT('',(-0.038018235775,0.010630560705,-0.019377346763));
#16844=CARTESIAN_POINT('',(-0.037508746133,0.010687144809,-0.019359690396));
#16845=CARTESIAN_POINT('',(-0.037758428154,0.010790336157,-0.019796053532));
#16846=CARTESIAN_POINT('',(-0.037983863425,0.010411968137,-0.019436057889));
#16847=CARTESIAN_POINT('',(-0.037485152239,0.010495505976,-0.019418486321));
#16848=CARTESIAN_POINT('',(-0.037724055805,0.010539762158,-0.019863756543));
#16849=CARTESIAN_POINT('',(-0.03795238138,0.010264782581,-0.019459321592));
#16850=CARTESIAN_POINT('',(-0.037463427014,0.010365206315,-0.0194459996));
#16851=CARTESIAN_POINT('',(-0.037692573758,0.010371083162,-0.019890768551));
#16852=CARTESIAN_POINT('',(-0.037902538675,0.010079089663,-0.019469374787));
#16853=CARTESIAN_POINT('',(-0.037427207905,0.010194849921,-0.0194650503));
#16854=CARTESIAN_POINT('',(-0.037642731053,0.010158316591,-0.019902820673));
#16855=CARTESIAN_POINT('',(-0.0378920119,0.010041777162,-0.019470420515));
#16856=CARTESIAN_POINT('',(-0.037419583631,0.010160752482,-0.019468052396));
#16857=CARTESIAN_POINT('',(-0.037632204279,0.010115566184,-0.019904130213));
#16858=CARTESIAN_POINT('',(-0.037870126119,0.009967782025,-0.019470585011));
#16859=CARTESIAN_POINT('',(-0.037403612981,0.010092740755,-0.019472397637));
#16860=CARTESIAN_POINT('',(-0.037610318498,0.01003079121,-0.019904547896));
#16861=CARTESIAN_POINT('',(-0.037858748966,0.009931022823,-0.019469712501));
#16862=CARTESIAN_POINT('',(-0.037395262434,0.010058774628,-0.019473761339));
#16863=CARTESIAN_POINT('',(-0.037598941345,0.009988678904,-0.019903666229));
#16864=CARTESIAN_POINT('',(-0.037823348421,0.009821438911,-0.019464328495));
#16865=CARTESIAN_POINT('',(-0.037369172913,0.009957259452,-0.01947541277));
#16866=CARTESIAN_POINT('',(-0.0375635408,0.009863142675,-0.019897861604));
#16867=CARTESIAN_POINT('',(-0.037798059306,0.009749306074,-0.019457057728));
#16868=CARTESIAN_POINT('',(-0.037350277137,0.009889495687,-0.019473344227));
#16869=CARTESIAN_POINT('',(-0.037538251684,0.009780517328,-0.019889787243));
#16870=CARTESIAN_POINT('',(-0.037744193093,0.009606821654,-0.019435479151));
#16871=CARTESIAN_POINT('',(-0.037309379895,0.00975396796899999,-0.019462636177));
#16872=CARTESIAN_POINT('',(-0.037484385472,0.009617322054,-0.019865602347));
#16873=CARTESIAN_POINT('',(-0.037715615604,0.009536470315,-0.019421170251));
#16874=CARTESIAN_POINT('',(-0.037287455068,0.00968630927800001,-0.019454099651));
#16875=CARTESIAN_POINT('',(-0.037455807983,0.00953675241,-0.019849490561));
#16876=CARTESIAN_POINT('',(-0.037670271841,0.009432272932,-0.019394506946));
#16877=CARTESIAN_POINT('',(-0.037251993154,0.009584454943,-0.019436123721));
#16878=CARTESIAN_POINT('',(-0.03741046422,0.009417432004,-0.019819385249));
#16879=CARTESIAN_POINT('',(-0.037654725402,0.009397729381,-0.019384735691));
#16880=CARTESIAN_POINT('',(-0.037239813053,0.00955062727099999,-0.01942931378));
#16881=CARTESIAN_POINT('',(-0.037394917781,0.009377876793,-0.019808341439));
#16882=CARTESIAN_POINT('',(-0.037623119912,0.009329767162,-0.019363680484));
#16883=CARTESIAN_POINT('',(-0.037214887215,0.00948368581700001,-0.019414133917));
#16884=CARTESIAN_POINT('',(-0.037363312291,0.00930005825,-0.019784524364));
#16885=CARTESIAN_POINT('',(-0.037607024828,0.009296262741,-0.019352376907));
#16886=CARTESIAN_POINT('',(-0.037202122033,0.009450493943,-0.019405766262));
#16887=CARTESIAN_POINT('',(-0.037347217206,0.009261696717,-0.019771728968));
#16888=CARTESIAN_POINT('',(-0.037525118351,0.009131050827,-0.019292111621));
#16889=CARTESIAN_POINT('',(-0.037137549676,0.009287907011,-0.019360578083));
#16890=CARTESIAN_POINT('',(-0.03726531073,0.009072543594,-0.019703469308));
#16891=CARTESIAN_POINT('',(-0.037455051799,0.009006209944,-0.019232012958));
#16892=CARTESIAN_POINT('',(-0.037080651573,0.009160611098,-0.01931215418));
#16893=CARTESIAN_POINT('',(-0.037195244178,0.008929642002,-0.01963527735));
#16894=CARTESIAN_POINT('',(-0.037343235527,0.00882937501,-0.019125190743));
#16895=CARTESIAN_POINT('',(-0.036986748025,0.008975129884,-0.019219634813));
#16896=CARTESIAN_POINT('',(-0.037083427906,0.008727272424,-0.019513936502));
#16897=CARTESIAN_POINT('',(-0.03730475018,0.008772089632,-0.019086679248));
#16898=CARTESIAN_POINT('',(-0.03695443279,0.00891491662900001,-0.019185945236));
#16899=CARTESIAN_POINT('',(-0.037044942559,0.008661723823,-0.019470171615));
#16900=CARTESIAN_POINT('',(-0.03722687049,0.008662929292,-0.019005550035));
#16901=CARTESIAN_POINT('',(-0.036888415857,0.008799116535,-0.019113533106));
#16902=CARTESIAN_POINT('',(-0.036967062869,0.008536835522,-0.01937794176));
#16903=CARTESIAN_POINT('',(-0.037187320072,0.008610791877,-0.018962790615));
#16904=CARTESIAN_POINT('',(-0.036854627768,0.008743216033,-0.019074796792));
#16905=CARTESIAN_POINT('',(-0.036927512451,0.008477195434,-0.019329315909));
#16906=CARTESIAN_POINT('',(-0.03706685504,0.008461415123,-0.018828228599));
#16907=CARTESIAN_POINT('',(-0.036751742399,0.008583033822,-0.018951988873));
#16908=CARTESIAN_POINT('',(-0.036807047419,0.008306352736,-0.019176249766));
#16909=CARTESIAN_POINT('',(-0.03698413842,0.00837115601,-0.018730193296));
#16910=CARTESIAN_POINT('',(-0.036679594089,0.008483158251,-0.018859845872));
#16911=CARTESIAN_POINT('',(-0.036724330798,0.008203164137,-0.019064679358));
#16912=CARTESIAN_POINT('',(-0.036813690053,0.008209181877,-0.018517719676));
#16913=CARTESIAN_POINT('',(-0.036528822624,0.008301119021,-0.018655023827));
#16914=CARTESIAN_POINT('',(-0.036553882432,0.008018087581,-0.018822772918));
#16915=CARTESIAN_POINT('',(-0.03672806298,0.008139470644,-0.018405905936));
#16916=CARTESIAN_POINT('',(-0.036452219097,0.00822060741400001,-0.018545456308));
#16917=CARTESIAN_POINT('',(-0.036468255359,0.007938489295,-0.018695425021));
#16918=CARTESIAN_POINT('',(-0.036556082968,0.008021465132,-0.01817201132));
#16919=CARTESIAN_POINT('',(-0.036296957641,0.00808193927900001,-0.018312490038));
#16920=CARTESIAN_POINT('',(-0.036296275347,0.00780388162,-0.018428951735));
#16921=CARTESIAN_POINT('',(-0.036469700557,0.007973146042,-0.018049892539));
#16922=CARTESIAN_POINT('',(-0.036218299035,0.008023023348,-0.018189430236));
#16923=CARTESIAN_POINT('',(-0.03620989256,0.007748843646,-0.018289782591));
#16924=CARTESIAN_POINT('',(-0.0363829297,0.007935966222,-0.017922392252));
#16925=CARTESIAN_POINT('',(-0.036137554584,0.007975350095,-0.01805745087));
#16926=CARTESIAN_POINT('',(-0.036123122079,0.007706601765,-0.018144438831));
#16927=CARTESIAN_POINT('',(-0.0387712812904561,1.29142889886801E-11,-1.90090771351648E-11));
#16928=CARTESIAN_POINT('',(-0.0363829297,0.019489230098,-0.002088447775));
#16929=CARTESIAN_POINT('',(-0.036137554584,0.019625886228,-0.002121869649));
#16930=CARTESIAN_POINT('',(-0.036123122079,0.019566845848,-0.00239810651));
#16931=CARTESIAN_POINT('',(-0.036296388628,0.019360563338,-0.002056979854));
#16932=CARTESIAN_POINT('',(-0.036059352191,0.019492100962,-0.002097943941));
#16933=CARTESIAN_POINT('',(-0.03603658062,0.019420241494,-0.00236211242));
#16934=CARTESIAN_POINT('',(-0.036211750879,0.019236205228,-0.002014072051));
#16935=CARTESIAN_POINT('',(-0.03598108599,0.019359587151,-0.002061252005));
#16936=CARTESIAN_POINT('',(-0.035951943258,0.019278561257,-0.002312976363));
#16937=CARTESIAN_POINT('',(-0.036046427611,0.01899593144,-0.001905705907));
#16938=CARTESIAN_POINT('',(-0.03582764111,0.019102466172,-0.00196200056));
#16939=CARTESIAN_POINT('',(-0.03578661999,0.019004843948,-0.002188783069));
#16940=CARTESIAN_POINT('',(-0.035965731891,0.018880003958,-0.001840264492));
#16941=CARTESIAN_POINT('',(-0.035752240428,0.018977419333,-0.001900058743));
#16942=CARTESIAN_POINT('',(-0.03570592427,0.018872794113,-0.002113745518));
#16943=CARTESIAN_POINT('',(-0.035867783855,0.018740766939,-0.001742981965));
#16944=CARTESIAN_POINT('',(-0.035659677357,0.018825445883,-0.00180418218));
#16945=CARTESIAN_POINT('',(-0.035607976234,0.018714208906,-0.002002145766));
#16946=CARTESIAN_POINT('',(-0.03584830488,0.018713153198,-0.001722699015));
#16947=CARTESIAN_POINT('',(-0.035641412325,0.018795533693,-0.001784265567));
#16948=CARTESIAN_POINT('',(-0.035588497259,0.018682758826,-0.001978875521));
#16949=CARTESIAN_POINT('',(-0.035810061793,0.018659082064,-0.0016809538));
#16950=CARTESIAN_POINT('',(-0.035605524332,0.018736905391,-0.0017430598));
#16951=CARTESIAN_POINT('',(-0.035550254172,0.018621177248,-0.001930977518));
#16952=CARTESIAN_POINT('',(-0.035791254693,0.018632563266,-0.001659452537));
#16953=CARTESIAN_POINT('',(-0.035587855191,0.018708112389,-0.001721737929));
#16954=CARTESIAN_POINT('',(-0.035531447072,0.018590975808,-0.001906305033));
#16955=CARTESIAN_POINT('',(-0.035735788251,0.018554552292,-0.001593061423));
#16956=CARTESIAN_POINT('',(-0.035535852231,0.018623571688,-0.001655788575));
#16957=CARTESIAN_POINT('',(-0.03547598063,0.018502133765,-0.001830115341));
#16958=CARTESIAN_POINT('',(-0.035700081089,0.018504601769,-0.00154628902));
#16959=CARTESIAN_POINT('',(-0.035502196601,0.018569127867,-0.001608840169));
#16960=CARTESIAN_POINT('',(-0.035440273468,0.018445251153,-0.001776431383));
#16961=CARTESIAN_POINT('',(-0.035596955729,0.01836101404,-0.001398258712));
#16962=CARTESIAN_POINT('',(-0.035405412743,0.018413252525,-0.001459938607));
#16963=CARTESIAN_POINT('',(-0.035337148108,0.018281744346,-0.001606500757));
#16964=CARTESIAN_POINT('',(-0.035533471872,0.018273557744,-0.001289394297));
#16965=CARTESIAN_POINT('',(-0.03534514464,0.018317127379,-0.001348630596));
#16966=CARTESIAN_POINT('',(-0.035273664252,0.018182166802,-0.001481497731));
#16967=CARTESIAN_POINT('',(-0.035462076716,0.01817592941,-0.001138664356));
#16968=CARTESIAN_POINT('',(-0.035277056499,0.018209299086,-0.001192172175));
#16969=CARTESIAN_POINT('',(-0.035202269094,0.018071016536,-0.001308380108));
#16970=CARTESIAN_POINT('',(-0.035448157312,0.018156936087,-0.00110767252));
#16971=CARTESIAN_POINT('',(-0.035263851039,0.018188427631,-0.001160131862));
#16972=CARTESIAN_POINT('',(-0.035188349691,0.018049393067,-0.001272783163));
#16973=CARTESIAN_POINT('',(-0.035421421576,0.018120522953,-0.001044695664));
#16974=CARTESIAN_POINT('',(-0.035238481118,0.01814840061,-0.001094908468));
#16975=CARTESIAN_POINT('',(-0.035161613954,0.018007938413,-0.001200444691));
#16976=CARTESIAN_POINT('',(-0.035408615027,0.01810311612,-0.001012747602));
#16977=CARTESIAN_POINT('',(-0.035226318844,0.018129247863,-0.001061759551));
#16978=CARTESIAN_POINT('',(-0.035148807406,0.017988121995,-0.001163745631));
#16979=CARTESIAN_POINT('',(-0.035371903227,0.018053301561,-0.000915516155));
#16980=CARTESIAN_POINT('',(-0.035191509303,0.018074518308,-0.000960895819));
#16981=CARTESIAN_POINT('',(-0.035112095605,0.01793141283,-0.001052049584));
#16982=CARTESIAN_POINT('',(-0.035349701075,0.018023292834,-0.000848849473));
#16983=CARTESIAN_POINT('',(-0.035170375015,0.018041410365,-0.000891381795));
#16984=CARTESIAN_POINT('',(-0.035089893455,0.017897252254,-0.000975458269));
#16985=CARTESIAN_POINT('',(-0.035310076825,0.017969873141,-0.000711689247));
#16986=CARTESIAN_POINT('',(-0.035132682741,0.01798250627,-0.00074809069));
#16987=CARTESIAN_POINT('',(-0.035050269204,0.01783644352,-0.000817866864));
#16988=CARTESIAN_POINT('',(-0.035292653375,0.01794646038,-0.000641196756));
#16989=CARTESIAN_POINT('',(-0.035116074086,0.017956629983,-0.000674242814));
#16990=CARTESIAN_POINT('',(-0.035032845755,0.017809793311,-0.000736867981));
#16991=CARTESIAN_POINT('',(-0.035270404132,0.017916617409,-0.000532382892));
#16992=CARTESIAN_POINT('',(-0.035094864144,0.017923641781,-0.000560006423));
#16993=CARTESIAN_POINT('',(-0.03501059651,0.017775824484,-0.00061182896));
#16994=CARTESIAN_POINT('',(-0.03526362249,0.017907532057,-0.000495486354));
#16995=CARTESIAN_POINT('',(-0.035088401673,0.017913601835,-0.000521272544));
#16996=CARTESIAN_POINT('',(-0.035003814869,0.017765483208,-0.000569429626));
#16997=CARTESIAN_POINT('',(-0.035251577427,0.017891408044,-0.000421626354));
#16998=CARTESIAN_POINT('',(-0.035076925826,0.017895786451,-0.000443697364));
#16999=CARTESIAN_POINT('',(-0.034991769806,0.017747130448,-0.000484552102));
#17000=CARTESIAN_POINT('',(-0.035246291308,0.01788433888,-0.000384573767));
#17001=CARTESIAN_POINT('',(-0.035071886429,0.017887970471,-0.000404748673));
#17002=CARTESIAN_POINT('',(-0.034986483687,0.017739084243,-0.000441971503));
#17003=CARTESIAN_POINT('',(-0.035223521483,0.017853905806,-0.00019870341));
#17004=CARTESIAN_POINT('',(-0.035050225188,0.017854392227,-0.000209670015));
#17005=CARTESIAN_POINT('',(-0.034963713862,0.017704445198,-0.000228366787));
#17006=CARTESIAN_POINT('',(-0.035216913712,0.017845112687,-4.808316E-5));
#17007=CARTESIAN_POINT('',(-0.035043883179,0.017844601077,-5.0495546E-5));
#17008=CARTESIAN_POINT('',(-0.034957106091,0.017694437363,-5.5260102E-5));
#17009=CARTESIAN_POINT('',(-0.035223876434,0.017854401084,0.000142705112));
#17010=CARTESIAN_POINT('',(-0.035050518048,0.017854867848,0.00015026669));
#17011=CARTESIAN_POINT('',(-0.034964068813,0.017705009213,0.000164006944));
#17012=CARTESIAN_POINT('',(-0.03522604562,0.017857295098,0.000181008826));
#17013=CARTESIAN_POINT('',(-0.035052587043,0.017858069693,0.000190597666));
#17014=CARTESIAN_POINT('',(-0.034966237999,0.01770830312,0.000208027982));
#17015=CARTESIAN_POINT('',(-0.035231850552,0.017865043926,0.000256731481));
#17016=CARTESIAN_POINT('',(-0.035058120997,0.017866638035,0.000270288381));
#17017=CARTESIAN_POINT('',(-0.034972042931,0.017717122731,0.00029505227));
#17018=CARTESIAN_POINT('',(-0.0352354894,0.01786990288,0.000294294755));
#17019=CARTESIAN_POINT('',(-0.035061591095,0.017872012494,0.000309815542));
#17020=CARTESIAN_POINT('',(-0.034975681779,0.01772265315,0.0003382214));
#17021=CARTESIAN_POINT('',(-0.035248550352,0.017887356278,0.000406114618));
#17022=CARTESIAN_POINT('',(-0.035074046816,0.017891317393,0.000427475545));
#17023=CARTESIAN_POINT('',(-0.034988742731,0.01774251863,0.000466726903));
#17024=CARTESIAN_POINT('',(-0.035260111701,0.017902819307,0.000479503556));
#17025=CARTESIAN_POINT('',(-0.035085080525,0.017908432544,0.000504635436));
#17026=CARTESIAN_POINT('',(-0.03500030408,0.017760118859,0.000551064032));
#17027=CARTESIAN_POINT('',(-0.035281577861,0.017931602322,0.000587901928));
#17028=CARTESIAN_POINT('',(-0.035105505104,0.017940189326,0.000618239168));
#17029=CARTESIAN_POINT('',(-0.03502177024,0.017792881061,0.000675626671));
#17030=CARTESIAN_POINT('',(-0.035289421938,0.017942130116,0.000623753285));
#17031=CARTESIAN_POINT('',(-0.035112977015,0.017951817298,0.000655825409));
#17032=CARTESIAN_POINT('',(-0.035029614317,0.017804864435,0.000716823028));
#17033=CARTESIAN_POINT('',(-0.035306476701,0.017965050902,0.000694894802));
#17034=CARTESIAN_POINT('',(-0.035129211644,0.017977114049,0.000730326682));
#17035=CARTESIAN_POINT('',(-0.03504666908,0.017830954681,0.000798568263));
#17036=CARTESIAN_POINT('',(-0.035315718145,0.017977485365,0.000730290044));
#17037=CARTESIAN_POINT('',(-0.035138009535,0.017990837846,0.000767363366));
#17038=CARTESIAN_POINT('',(-0.035055910524,0.017845108762,0.000839237874));
#17039=CARTESIAN_POINT('',(-0.035345244257,0.018017274364,0.000834778442));
#17040=CARTESIAN_POINT('',(-0.035166136457,0.018034776161,0.000876705266000001));
#17041=CARTESIAN_POINT('',(-0.035085436637,0.017890401172,0.000959292019));
#17042=CARTESIAN_POINT('',(-0.035367258146,0.018047016063,0.000902026906));
#17043=CARTESIAN_POINT('',(-0.035187092355,0.018067591645,0.000946845463));
#17044=CARTESIAN_POINT('',(-0.035107450524,0.017924257611,0.001036552565));
#17045=CARTESIAN_POINT('',(-0.035415540032,0.01811249853,0.001032054747));
#17046=CARTESIAN_POINT('',(-0.035232955499,0.018139667727,0.001082015991));
#17047=CARTESIAN_POINT('',(-0.035155732411,0.017998802798,0.001185925847));
#17048=CARTESIAN_POINT('',(-0.035441809443,0.018148241136,0.001094832722));
#17049=CARTESIAN_POINT('',(-0.035257918294,0.018179017227,0.001147092497));
#17050=CARTESIAN_POINT('',(-0.035182001822,0.018039493646,0.001258036973));
#17051=CARTESIAN_POINT('',(-0.035498359317,0.018225522805,0.001216100433));
#17052=CARTESIAN_POINT('',(-0.035311533473,0.018263877422,0.001272286645));
#17053=CARTESIAN_POINT('',(-0.035238551696,0.018127478563,0.001397318651));
#17054=CARTESIAN_POINT('',(-0.035528803299,0.018267288112,0.001274848098));
#17055=CARTESIAN_POINT('',(-0.035340397738,0.018309728944,0.001332693764));
#17056=CARTESIAN_POINT('',(-0.035268995678,0.01817503025,0.001464785336));
#17057=CARTESIAN_POINT('',(-0.035624302868,0.018398937175,0.001441946764));
#17058=CARTESIAN_POINT('',(-0.035431143853,0.018454527567,0.001504443888));
#17059=CARTESIAN_POINT('',(-0.035364495247,0.018324926454,0.001656660391));
#17060=CARTESIAN_POINT('',(-0.035693625065,0.018495301896,0.001541838752));
#17061=CARTESIAN_POINT('',(-0.035496770299,0.018560086634,0.001605426885));
#17062=CARTESIAN_POINT('',(-0.035433817443,0.018434657594,0.001771331198));
#17063=CARTESIAN_POINT('',(-0.035804878296,0.018651701588,0.001676100287));
#17064=CARTESIAN_POINT('',(-0.035600812464,0.018729153932,0.001738536628));
#17065=CARTESIAN_POINT('',(-0.035545070675,0.018612771043,0.001925410518));
#17066=CARTESIAN_POINT('',(-0.035843360668,0.01870607504,0.001718396961));
#17067=CARTESIAN_POINT('',(-0.035636958249,0.018788171317,0.001780300456));
#17068=CARTESIAN_POINT('',(-0.035583553047,0.018674696557,0.001973941769));
#17069=CARTESIAN_POINT('',(-0.035921655233,0.018817323726,0.001796776766));
#17070=CARTESIAN_POINT('',(-0.035710302083,0.018908539739,0.001856931323));
#17071=CARTESIAN_POINT('',(-0.035661847612,0.018801403665,0.002063858322));
#17072=CARTESIAN_POINT('',(-0.035961464931,0.018874192105,0.001832902387));
#17073=CARTESIAN_POINT('',(-0.035747535996,0.018969953338,0.00189179072));
#17074=CARTESIAN_POINT('',(-0.035701657309,0.018866177417,0.002105292476));
#17075=CARTESIAN_POINT('',(-0.036082708725,0.019048372444,0.001932563921));
#17076=CARTESIAN_POINT('',(-0.035861344783,0.019158636987,0.001987306041));
#17077=CARTESIAN_POINT('',(-0.035822901104,0.019064581187,0.00221957399));
#17078=CARTESIAN_POINT('',(-0.036165937985,0.019169231525,0.001987458368));
#17079=CARTESIAN_POINT('',(-0.035938765603,0.019288313365,0.002037355517));
#17080=CARTESIAN_POINT('',(-0.035906130364,0.019202261747,0.00228248524));
#17081=CARTESIAN_POINT('',(-0.036272749616,0.019326186492,0.002041954834));
#17082=CARTESIAN_POINT('',(-0.036036325391,0.019453445768,0.002083965382));
#17083=CARTESIAN_POINT('',(-0.036012941995,0.019381080036,0.002344895831));
#17084=CARTESIAN_POINT('',(-0.036294271622,0.019357902787,0.002052147118));
#17085=CARTESIAN_POINT('',(-0.036056160144,0.019487107185,0.002092585706));
#17086=CARTESIAN_POINT('',(-0.036034464001,0.019417215175,0.002356565423));
#17087=CARTESIAN_POINT('',(-0.036337241164,0.019421408713,0.002070948756));
#17088=CARTESIAN_POINT('',(-0.036095695252,0.019554376812,0.002108113551));
#17089=CARTESIAN_POINT('',(-0.036077433543,0.019489570721,0.002378086456));
#17090=CARTESIAN_POINT('',(-0.036358730845,0.019453260076,0.002079581263));
#17091=CARTESIAN_POINT('',(-0.03611543566,0.019588053885,0.00211503004));
#17092=CARTESIAN_POINT('',(-0.036098923223,0.019525861458,0.002387964418));
#17093=CARTESIAN_POINT('',(-0.036423211553,0.019549105164,0.002103217759));
#17094=CARTESIAN_POINT('',(-0.036174782484,0.019689559821,0.002133392794));
#17095=CARTESIAN_POINT('',(-0.036163403931,0.019635067732,0.002415001427));
#17096=CARTESIAN_POINT('',(-0.036466213928,0.019613389425,0.002115965485));
#17097=CARTESIAN_POINT('',(-0.036214084658,0.01975713597,0.002142252449));
#17098=CARTESIAN_POINT('',(-0.036206406307,0.019708316806,0.002429569065));
#17099=CARTESIAN_POINT('',(-0.036595254777,0.019807388917,0.002145346512));
#17100=CARTESIAN_POINT('',(-0.03633245937,0.019961690258,0.002159474874));
#17101=CARTESIAN_POINT('',(-0.036335447156,0.019929380277,0.002463096114));
#17102=CARTESIAN_POINT('',(-0.036681322249,0.019938243356,0.002153193167));
#17103=CARTESIAN_POINT('',(-0.036410235723,0.020097509831,0.00215769725));
#17104=CARTESIAN_POINT('',(-0.036421514628,0.020078502366,0.002471966356));
#17105=CARTESIAN_POINT('',(-0.03678899075,0.020103771553,0.002147749667));
#17106=CARTESIAN_POINT('',(-0.036505370032,0.020265213313,0.002139955671));
#17107=CARTESIAN_POINT('',(-0.036529183129,0.02026715354,0.002465549917));
#17108=CARTESIAN_POINT('',(-0.036810556304,0.020137018306,0.002145885901));
#17109=CARTESIAN_POINT('',(-0.036524605066,0.020299204976,0.002135530565));
#17110=CARTESIAN_POINT('',(-0.036550748683,0.020305045337,0.002463377054));
#17111=CARTESIAN_POINT('',(-0.036853337272,0.020203152393,0.00214063762));
#17112=CARTESIAN_POINT('',(-0.036562661331,0.020366616451,0.002125129214));
#17113=CARTESIAN_POINT('',(-0.036593529651,0.020380420704,0.002457286744));
#17114=CARTESIAN_POINT('',(-0.036874593816,0.020236102715,0.002137253074));
#17115=CARTESIAN_POINT('',(-0.036581516731,0.020400097569,0.002119135437));
#17116=CARTESIAN_POINT('',(-0.036614786195,0.020417976062,0.002453369195));
#17117=CARTESIAN_POINT('',(-0.036937968442,0.020334604047,0.002124834324));
#17118=CARTESIAN_POINT('',(-0.03663781018,0.020500286578,0.002098765055));
#17119=CARTESIAN_POINT('',(-0.03667816082,0.020530245644,0.002439018114));
#17120=CARTESIAN_POINT('',(-0.03697969206,0.020399806189,0.002113539669));
#17121=CARTESIAN_POINT('',(-0.036674489896,0.020565883365,0.002082096496));
#17122=CARTESIAN_POINT('',(-0.036719884461,0.020604564293,0.002425991486));
#17123=CARTESIAN_POINT('',(-0.037020900622,0.020464534491,0.002099215974));
#17124=CARTESIAN_POINT('',(-0.036710197303,0.02063001576,0.002062596704));
#17125=CARTESIAN_POINT('',(-0.036761093001,0.0206783452,0.002409490732));
#17126=CARTESIAN_POINT('',(-0.0370209006221877,0.0205293532570174,0.00239212983048223));
#17127=CARTESIAN_POINT('',(-0.0363829297001963,0.019417959879229,-0.00237985909232116));
#17128=CARTESIAN_POINT('',(-0.0370209006725265,0.0204645345703645,0.00209921595643747));
#17129=CARTESIAN_POINT('',(-0.0367101973471479,0.0206300158392919,0.00206259667989087));
#17130=CARTESIAN_POINT('',(-0.0367610930515268,0.0206783452904645,0.00240949071176802));
#17131=CARTESIAN_POINT('',(-0.037103317012847,0.0205939899421424,0.00207056883537586));
#17132=CARTESIAN_POINT('',(-0.0367834353017993,0.0207615550854043,0.00202260147516363));
#17133=CARTESIAN_POINT('',(-0.0368435097848469,0.0208259064844385,0.00237648933787403));
#17134=CARTESIAN_POINT('',(-0.0371836845969985,0.0207215678876372,0.00202989413701114));
#17135=CARTESIAN_POINT('',(-0.036852619292111,0.0208869959479472,0.00197074610137332));
#17136=CARTESIAN_POINT('',(-0.0369238769759985,0.0209713360532264,0.00232969336136768));
#17137=CARTESIAN_POINT('',(-0.037301116085,0.020909749705,0.001949233973));
#17138=CARTESIAN_POINT('',(-0.03695137278,0.021067368688,0.001875640572));
#17139=CARTESIAN_POINT('',(-0.037041308464,0.021185862625,0.002236969898));
#17140=CARTESIAN_POINT('',(-0.037339424126,0.020971441729,0.001919241095));
#17141=CARTESIAN_POINT('',(-0.036983551057,0.021126386976,0.001840720983));
#17142=CARTESIAN_POINT('',(-0.037079616505,0.021256193347,0.002202501046));
#17143=CARTESIAN_POINT('',(-0.037413681214,0.021091557342,0.001853560892));
#17144=CARTESIAN_POINT('',(-0.037045412802,0.021240237534,0.00176594903));
#17145=CARTESIAN_POINT('',(-0.037153873593,0.021393132117,0.002127037152));
#17146=CARTESIAN_POINT('',(-0.037449744946,0.021150164712,0.001817796718));
#17147=CARTESIAN_POINT('',(-0.037075133644,0.021295144276,0.001725939277));
#17148=CARTESIAN_POINT('',(-0.037189937325,0.021459949676,0.002085953763));
#17149=CARTESIAN_POINT('',(-0.037519742735,0.021264387507,0.001740283886));
#17150=CARTESIAN_POINT('',(-0.037132298021,0.021401075383,0.001640887915));
#17151=CARTESIAN_POINT('',(-0.037259935114,0.021590176641,0.001996928158));
#17152=CARTESIAN_POINT('',(-0.037553677068,0.021320003507,0.001698536285));
#17153=CARTESIAN_POINT('',(-0.037159681014,0.02145199347,0.001595792365));
#17154=CARTESIAN_POINT('',(-0.037293869447,0.021653586706,0.001948987157));
#17155=CARTESIAN_POINT('',(-0.037602938649,0.021401048787,0.001631194651));
#17156=CARTESIAN_POINT('',(-0.037198872381,0.02152506771,0.00152463845));
#17157=CARTESIAN_POINT('',(-0.037343131027,0.021745991586,0.001871665827));
#17158=CARTESIAN_POINT('',(-0.037619085386,0.02142766668,0.001607959283));
#17159=CARTESIAN_POINT('',(-0.037211691522,0.021549005368,0.00150017865));
#17160=CARTESIAN_POINT('',(-0.037359277765,0.02177634066,0.00184498875));
#17161=CARTESIAN_POINT('',(-0.037650817756,0.021480075164,0.001559853428));
#17162=CARTESIAN_POINT('',(-0.037236742776,0.021595846177,0.001449961208));
#17163=CARTESIAN_POINT('',(-0.037391010135,0.021836096115,0.001789760567));
#17164=CARTESIAN_POINT('',(-0.037666411882,0.021505880156,0.001534959604));
#17165=CARTESIAN_POINT('',(-0.037248972401,0.021618745415,0.001424178176));
#17166=CARTESIAN_POINT('',(-0.037406604261,0.02186551892,0.001761182687));
#17167=CARTESIAN_POINT('',(-0.037742059103,0.021631281365,0.001407777533));
#17168=CARTESIAN_POINT('',(-0.037308672836,0.021730666169,0.001291938074));
#17169=CARTESIAN_POINT('',(-0.037482251481,0.022008502436,0.001615186583));
#17170=CARTESIAN_POINT('',(-0.037795953594,0.021721337673,0.001296356849));
#17171=CARTESIAN_POINT('',(-0.037349209561,0.021807099305,0.001180907653));
#17172=CARTESIAN_POINT('',(-0.037536145973,0.022111189537,0.001487307464));
#17173=CARTESIAN_POINT('',(-0.037866774638,0.021840245218,0.001114117882));
#17174=CARTESIAN_POINT('',(-0.037401307565,0.021905583424,0.001005823865));
#17175=CARTESIAN_POINT('',(-0.037606967016,0.022246777496,0.001278179341));
#17176=CARTESIAN_POINT('',(-0.037888699602,0.021877166648,0.001050836305));
#17177=CARTESIAN_POINT('',(-0.037417279271,0.021935830648,0.000945510459000001));
#17178=CARTESIAN_POINT('',(-0.037628891981,0.022288878891,0.001205565251));
#17179=CARTESIAN_POINT('',(-0.037918925522,0.02192817688,0.000951846528));
#17180=CARTESIAN_POINT('',(-0.037439020962,0.02197705154,0.000852704956));
#17181=CARTESIAN_POINT('',(-0.037659117901,0.022347046289,0.001091983109));
#17182=CARTESIAN_POINT('',(-0.037928582819,0.021944495043,0.000918060305));
#17183=CARTESIAN_POINT('',(-0.037445936687,0.021990172249,0.000821156235));
#17184=CARTESIAN_POINT('',(-0.037668775198,0.022365654138,0.001053217373));
#17185=CARTESIAN_POINT('',(-0.037946745879,0.021975216494,0.000849950291));
#17186=CARTESIAN_POINT('',(-0.037458875717,0.022014733087,0.000757954616));
#17187=CARTESIAN_POINT('',(-0.037686938258,0.022400686439,0.000975070946));
#17188=CARTESIAN_POINT('',(-0.03795527555,0.021989660009,0.000815562116));
#17189=CARTESIAN_POINT('',(-0.037464908394,0.022026190993,0.000726256116));
#17190=CARTESIAN_POINT('',(-0.037695467929,0.022417156761,0.000935616373));
#17191=CARTESIAN_POINT('',(-0.037995201404,0.022057326114,0.000641970034));
#17192=CARTESIAN_POINT('',(-0.037493219634,0.022079985093,0.000565981045));
#17193=CARTESIAN_POINT('',(-0.037735393783,0.022494318522,0.000736453018));
#17194=CARTESIAN_POINT('',(-0.03801852767,0.022097046697,0.000497868621));
#17195=CARTESIAN_POINT('',(-0.037508976952,0.022109994265,0.000437585608));
#17196=CARTESIAN_POINT('',(-0.037758720049,0.022539614123,0.000571137177));
#17197=CARTESIAN_POINT('',(-0.038040144091,0.022133880348,0.000273494358));
#17198=CARTESIAN_POINT('',(-0.037523624808,0.022137893532,0.000239691086));
#17199=CARTESIAN_POINT('',(-0.03778033647,0.022581617712,0.000313739898));
#17200=CARTESIAN_POINT('',(-0.038045091154,0.022142319282,0.000196876647));
#17201=CARTESIAN_POINT('',(-0.037526947936,0.022144225738,0.000172467167));
#17202=CARTESIAN_POINT('',(-0.037785283533,0.022591241175,0.000225847199));
#17203=CARTESIAN_POINT('',(-0.038050108278,0.022150877972,4.490289E-5));
#17204=CARTESIAN_POINT('',(-0.037530327064,0.02215066466,3.9232862E-5));
#17205=CARTESIAN_POINT('',(-0.037790300657,0.022601001208,5.1510166E-5));
#17206=CARTESIAN_POINT('',(-0.038050243047,0.022151108018,-3.0848498E-5));
#17207=CARTESIAN_POINT('',(-0.037530417095,0.022150836255,-2.6937103E-5));
#17208=CARTESIAN_POINT('',(-0.037790435426,0.022601263544,-3.5387705E-5));
#17209=CARTESIAN_POINT('',(-0.038045857381,0.022143626267,-0.000181889416));
#17210=CARTESIAN_POINT('',(-0.037527464034,0.022145209129,-0.0001593195));
#17211=CARTESIAN_POINT('',(-0.03778604976,0.022592731617,-0.000208654509));
#17212=CARTESIAN_POINT('',(-0.038041336883,0.022135914342,-0.000257178939));
#17213=CARTESIAN_POINT('',(-0.037524429559,0.022139426771,-0.000225336654));
#17214=CARTESIAN_POINT('',(-0.037781529262,0.022583937206,-0.00029502343));
#17215=CARTESIAN_POINT('',(-0.038027559938,0.022112436159,-0.000407289281));
#17216=CARTESIAN_POINT('',(-0.037515080889,0.022121619859,-0.000357917185));
#17217=CARTESIAN_POINT('',(-0.037767752317,0.022557163628,-0.000467226346));
#17218=CARTESIAN_POINT('',(-0.038018235775,0.022096554907,-0.000482337755));
#17219=CARTESIAN_POINT('',(-0.037508746133,0.022109556097,-0.0004245063));
#17220=CARTESIAN_POINT('',(-0.037758428154,0.022539053331,-0.000553321539));
#17221=CARTESIAN_POINT('',(-0.037983863425,0.02203810395,-0.000701000035));
#17222=CARTESIAN_POINT('',(-0.037485152239,0.022064655445,-0.00061986836));
#17223=CARTESIAN_POINT('',(-0.037724055805,0.02247239886,-0.000804176493));
#17224=CARTESIAN_POINT('',(-0.03795238138,0.02198465813,-0.000840098316));
#17225=CARTESIAN_POINT('',(-0.037463427014,0.022023332813,-0.000746467815999999));
#17226=CARTESIAN_POINT('',(-0.037692573758,0.022411452447,-0.000963762793));
#17227=CARTESIAN_POINT('',(-0.037902538675,0.021900517993,-0.001005939698));
#17228=CARTESIAN_POINT('',(-0.037427207905,0.021954653006,-0.000903526131000001));
#17229=CARTESIAN_POINT('',(-0.037642731053,0.022315506605,-0.001154050109));
#17230=CARTESIAN_POINT('',(-0.0378920119,0.021882767369,-0.001038776136));
#17231=CARTESIAN_POINT('',(-0.037419583631,0.021940204178,-0.000934556427));
#17232=CARTESIAN_POINT('',(-0.037632204279,0.022295265496,-0.001191727817));
#17233=CARTESIAN_POINT('',(-0.037870126119,0.021845912259,-0.001102940053));
#17234=CARTESIAN_POINT('',(-0.037403612981,0.021909961403,-0.000995628931000001));
#17235=CARTESIAN_POINT('',(-0.037610318498,0.022253239734,-0.00126535394));
#17236=CARTESIAN_POINT('',(-0.037858748966,0.021826777042,-0.001134338201));
#17237=CARTESIAN_POINT('',(-0.037395262434,0.02189415934,-0.001025726311));
#17238=CARTESIAN_POINT('',(-0.037598941345,0.022231420035,-0.001301383433));
#17239=CARTESIAN_POINT('',(-0.037823348421,0.0217673224,-0.001226548649));
#17240=CARTESIAN_POINT('',(-0.037369172913,0.021844831934,-0.001114466748));
#17241=CARTESIAN_POINT('',(-0.0375635408,0.022163624967,-0.001407198685));
#17242=CARTESIAN_POINT('',(-0.037798059306,0.021724959312,-0.001285382135));
#17243=CARTESIAN_POINT('',(-0.037350277137,0.02180915864,-0.001172117618));
#17244=CARTESIAN_POINT('',(-0.037538251684,0.022115319692,-0.001474717154));
#17245=CARTESIAN_POINT('',(-0.037744193093,0.021635029507,-0.001397987973));
#17246=CARTESIAN_POINT('',(-0.037309379895,0.021732121338,-0.001284134039));
#17247=CARTESIAN_POINT('',(-0.037484385472,0.022012777321,-0.001603955958));
#17248=CARTESIAN_POINT('',(-0.037715615604,0.021587461967,-0.00145175957));
#17249=CARTESIAN_POINT('',(-0.037287455068,0.021690899144,-0.001338459922));
#17250=CARTESIAN_POINT('',(-0.037455807983,0.021958539283,-0.001665675424));
#17251=CARTESIAN_POINT('',(-0.037670271841,0.021512272175,-0.001528665498));
#17252=CARTESIAN_POINT('',(-0.037251993154,0.021624404365,-0.001417680399));
#17253=CARTESIAN_POINT('',(-0.03741046422,0.021872807115,-0.001753957271));
#17254=CARTESIAN_POINT('',(-0.037654725402,0.021486538245,-0.001553695464));
#17255=CARTESIAN_POINT('',(-0.037239813053,0.021601592947,-0.001443571051));
#17256=CARTESIAN_POINT('',(-0.037394917781,0.021843465289,-0.001782691183));
#17257=CARTESIAN_POINT('',(-0.037623119912,0.02143432279,-0.001602024868));
#17258=CARTESIAN_POINT('',(-0.037214887215,0.021554976073,-0.00149395412));
#17259=CARTESIAN_POINT('',(-0.037363312291,0.021783929826,-0.001838175481));
#17260=CARTESIAN_POINT('',(-0.037607024828,0.021407781395,-0.001625388759));
#17261=CARTESIAN_POINT('',(-0.037202122033,0.021531133535,-0.001518515298));
#17262=CARTESIAN_POINT('',(-0.037347217206,0.021753667921,-0.001864999845));
#17263=CARTESIAN_POINT('',(-0.037525118351,0.02127298417,-0.001738333831));
#17264=CARTESIAN_POINT('',(-0.037137549676,0.021410705958,-0.001636725622));
#17265=CARTESIAN_POINT('',(-0.03726531073,0.02159997676,-0.001994681424));
#17266=CARTESIAN_POINT('',(-0.037455051799,0.02115851676,-0.001816399876));
#17267=CARTESIAN_POINT('',(-0.037080651573,0.021305121671,-0.001722755165));
#17268=CARTESIAN_POINT('',(-0.037195244178,0.021469469996,-0.002084341855));
#17269=CARTESIAN_POINT('',(-0.037343235527,0.020977588541,-0.001916132313));
#17270=CARTESIAN_POINT('',(-0.036986748025,0.021132256941,-0.001837126924));
#17271=CARTESIAN_POINT('',(-0.037083427906,0.021263200951,-0.002198928626));
#17272=CARTESIAN_POINT('',(-0.03730475018,0.020915593919,-0.001946487158));
#17273=CARTESIAN_POINT('',(-0.03695443279,0.021072974284,-0.001872428345));
#17274=CARTESIAN_POINT('',(-0.037044942559,0.021192525146,-0.002233812936));
#17275=CARTESIAN_POINT('',(-0.03722687049,0.020790753789,-0.002000458179));
#17276=CARTESIAN_POINT('',(-0.036888415857,0.020952363493,-0.001936508103));
#17277=CARTESIAN_POINT('',(-0.036967062869,0.021050207598,-0.00229585445));
#17278=CARTESIAN_POINT('',(-0.037187320072,0.020727654338,-0.002024230796));
#17279=CARTESIAN_POINT('',(-0.036854627768,0.020890866611,-0.001965551201));
#17280=CARTESIAN_POINT('',(-0.036927512451,0.020978276332,-0.002323191356));
#17281=CARTESIAN_POINT('',(-0.03706685504,0.020536431836,-0.002086313851));
#17282=CARTESIAN_POINT('',(-0.036751742399,0.020704420727,-0.002042869105));
#17283=CARTESIAN_POINT('',(-0.036807047419,0.020760295815,-0.0023946124));
#17284=CARTESIAN_POINT('',(-0.03698413842,0.020406401217,-0.002115462885));
#17285=CARTESIAN_POINT('',(-0.036679594089,0.020574684762,-0.002083292386));
#17286=CARTESIAN_POINT('',(-0.036724330798,0.020612078707,-0.002428191144));
#17287=CARTESIAN_POINT('',(-0.036813690053,0.020141406598,-0.002149499788));
#17288=CARTESIAN_POINT('',(-0.036528822624,0.020306284053,-0.002138531962));
#17289=CARTESIAN_POINT('',(-0.036553882432,0.020310043308,-0.002467518924));
#17290=CARTESIAN_POINT('',(-0.03672806298,0.020009717442,-0.002153964617));
#17291=CARTESIAN_POINT('',(-0.036452219097,0.020171139995,-0.002153473299));
#17292=CARTESIAN_POINT('',(-0.036468255359,0.020159957651,-0.002472779113));
#17293=CARTESIAN_POINT('',(-0.036556082968,0.019748156007,-0.00213921308));
#17294=CARTESIAN_POINT('',(-0.036296957641,0.019900051219,-0.002157080292));
#17295=CARTESIAN_POINT('',(-0.036296275347,0.019861881178,-0.002456116136));
#17296=CARTESIAN_POINT('',(-0.036469700557,0.019618238496,-0.002119999249));
#17297=CARTESIAN_POINT('',(-0.036218299035,0.019764020339,-0.002146573084));
#17298=CARTESIAN_POINT('',(-0.03620989256,0.019713838176,-0.002434195848));
#17299=CARTESIAN_POINT('',(-0.0363829297,0.019489230098,-0.002088447775));
#17300=CARTESIAN_POINT('',(-0.036137554584,0.019625886228,-0.002121869649));
#17301=CARTESIAN_POINT('',(-0.036123122079,0.019566845848,-0.00239810651));
#17302=CARTESIAN_POINT('',(-0.0387712812776768,1.75917299243037E-11,-4.54757954297462E-17));
#17303=CARTESIAN_POINT('',(-0.0385114725585428,0.0237182560306759,0.00250334555505273));
#17304=CARTESIAN_POINT('',(-0.0385732886842286,0.0238313054539707,0.00245233227695023));
#17305=CARTESIAN_POINT('',(-0.0386752801539392,0.0238844424604606,0.00235430274800211));
#17306=CARTESIAN_POINT('',(-0.0387712812922245,0.0238935321467088,0.00225812345823692));
#17307=CARTESIAN_POINT('',(-0.087860759494,0.023594862995,0.002229896915));
#17308=CARTESIAN_POINT('',(-0.0363829297,0.011553263876,0.015833944478));
#17309=CARTESIAN_POINT('',(-0.036137554584,0.011650536133,0.015935581221));
#17310=CARTESIAN_POINT('',(-0.036123122079,0.011860244082,0.015746332321));
#17311=CARTESIAN_POINT('',(-0.036296388628,0.011461678478,0.015738249755));
#17312=CARTESIAN_POINT('',(-0.036059352191,0.01156292323,0.015831682636));
#17313=CARTESIAN_POINT('',(-0.03603658062,0.011755770109,0.015637366271));
#17314=CARTESIAN_POINT('',(-0.036211750879,0.011362340175,0.015652006375));
#17315=CARTESIAN_POINT('',(-0.03598108599,0.011464890175,0.015735268277));
#17316=CARTESIAN_POINT('',(-0.035951943258,0.011642376917,0.015539235616));
#17317=CARTESIAN_POINT('',(-0.036046427611,0.011148355448,0.015498106242));
#17318=CARTESIAN_POINT('',(-0.03582764111,0.011250375413,0.0155622207));
#17319=CARTESIAN_POINT('',(-0.03578661999,0.011397963715,0.015364286119));
#17320=CARTESIAN_POINT('',(-0.035965731891,0.011033717779,0.015430430805));
#17321=CARTESIAN_POINT('',(-0.035752240428,0.011134208806,0.015484897869));
#17322=CARTESIAN_POINT('',(-0.03570592427,0.011266954373,0.015287446383));
#17323=CARTESIAN_POINT('',(-0.035867783855,0.01087985013,0.015358489273));
#17324=CARTESIAN_POINT('',(-0.035659677357,0.010975190542,0.015401223282));
#17325=CARTESIAN_POINT('',(-0.035607976234,0.011091013549,0.015205907441));
#17326=CARTESIAN_POINT('',(-0.03584830488,0.010848477709,0.015344716547));
#17327=CARTESIAN_POINT('',(-0.035641412325,0.010942986155,0.015385276872));
#17328=CARTESIAN_POINT('',(-0.035588497259,0.011055135885,0.015190305996));
#17329=CARTESIAN_POINT('',(-0.035810061793,0.010785289725,0.015318762179));
#17330=CARTESIAN_POINT('',(-0.035605524332,0.010877986763,0.015355106157));
#17331=CARTESIAN_POINT('',(-0.035550254172,0.010982864209,0.015160923786));
#17332=CARTESIAN_POINT('',(-0.035791254693,0.010753409687,0.015306546858));
#17333=CARTESIAN_POINT('',(-0.035587855191,0.01084512498,0.015340831622));
#17334=CARTESIAN_POINT('',(-0.035531447072,0.01094639649,0.015147104814));
#17335=CARTESIAN_POINT('',(-0.035735788251,0.010656907808,0.015272182929));
#17336=CARTESIAN_POINT('',(-0.035535852231,0.010745740813,0.015300591903));
#17337=CARTESIAN_POINT('',(-0.03547598063,0.01083599326,0.015108260194));
#17338=CARTESIAN_POINT('',(-0.035700081089,0.010591426457,0.015252310709));
#17339=CARTESIAN_POINT('',(-0.035502196601,0.010677860391,0.015276916375));
#17340=CARTESIAN_POINT('',(-0.035440273468,0.010761060282,0.015085840387));
#17341=CARTESIAN_POINT('',(-0.035596955729,0.010391434585,0.015201975242));
#17342=CARTESIAN_POINT('',(-0.035405412743,0.010470970184,0.015216375149));
#17343=CARTESIAN_POINT('',(-0.035337148108,0.01053214264,0.01502920465));
#17344=CARTESIAN_POINT('',(-0.035533471872,0.010253427089,0.015180668075));
#17345=CARTESIAN_POINT('',(-0.03534514464,0.010326512046,0.015188782336));
#17346=CARTESIAN_POINT('',(-0.035273664252,0.010374098072,0.015005469481));
#17347=CARTESIAN_POINT('',(-0.035462076716,0.010074076964,0.015171484429));
#17348=CARTESIAN_POINT('',(-0.035277056499,0.010137100933,0.015173629506));
#17349=CARTESIAN_POINT('',(-0.035202269094,0.01016859868,0.014995769339));
#17350=CARTESIAN_POINT('',(-0.035448157312,0.010037740585,0.015170531646));
#17351=CARTESIAN_POINT('',(-0.035263851039,0.01009891748,0.015171574453));
#17352=CARTESIAN_POINT('',(-0.035188349691,0.010126959086,0.014994841338));
#17353=CARTESIAN_POINT('',(-0.035421421576,0.009964994461,0.015170485375));
#17354=CARTESIAN_POINT('',(-0.035238481118,0.010022418853,0.015169521732));
#17355=CARTESIAN_POINT('',(-0.035161613954,0.010043584805,0.01499510979));
#17356=CARTESIAN_POINT('',(-0.035408615027,0.009928623211,0.015171384646));
#17357=CARTESIAN_POINT('',(-0.035226318844,0.009984134676,0.015169509426));
#17358=CARTESIAN_POINT('',(-0.035148807406,0.010001894278,0.014996297799));
#17359=CARTESIAN_POINT('',(-0.035371903227,0.009819511029,0.015176859697));
#17360=CARTESIAN_POINT('',(-0.035191509303,0.009869419344,0.015172544106));
#17361=CARTESIAN_POINT('',(-0.035112095605,0.00987680808,0.015003034244));
#17362=CARTESIAN_POINT('',(-0.035349701075,0.009746771624,0.015184204718));
#17363=CARTESIAN_POINT('',(-0.035170375015,0.009792664461,0.015178628799));
#17364=CARTESIAN_POINT('',(-0.035089893455,0.009793397768,0.015011745976));
#17365=CARTESIAN_POINT('',(-0.035310076825,0.009601277538,0.015206522019));
#17366=CARTESIAN_POINT('',(-0.035132682741,0.009639118677,0.015199261909));
#17367=CARTESIAN_POINT('',(-0.035050269204,0.009626515241,0.01503787977));
#17368=CARTESIAN_POINT('',(-0.035292653375,0.00952852287,0.015221492219));
#17369=CARTESIAN_POINT('',(-0.035116074086,0.009562226397,0.015213776324));
#17370=CARTESIAN_POINT('',(-0.035032845755,0.009543043046,0.015055299453));
#17371=CARTESIAN_POINT('',(-0.035270404132,0.009419365813,0.015250054381));
#17372=CARTESIAN_POINT('',(-0.035094864144,0.00944680067900001,0.015242325899));
#17373=CARTESIAN_POINT('',(-0.03501059651,0.009417771664,0.015088401097));
#17374=CARTESIAN_POINT('',(-0.03526362249,0.009382869798,0.015260634503));
#17375=CARTESIAN_POINT('',(-0.035088401673,0.009408236182,0.01525299799));
#17376=CARTESIAN_POINT('',(-0.035003814869,0.009375882126,0.015100644955));
#17377=CARTESIAN_POINT('',(-0.035251577427,0.009310843156,0.015283600698));
#17378=CARTESIAN_POINT('',(-0.035076925826,0.009332146415,0.015276357005));
#17379=CARTESIAN_POINT('',(-0.034991769806,0.009293199654,0.015127189761));
#17380=CARTESIAN_POINT('',(-0.035246291308,0.009275220092,0.015296004916));
#17381=CARTESIAN_POINT('',(-0.035071886429,0.009294507868,0.015289062514));
#17382=CARTESIAN_POINT('',(-0.034986483687,0.009252300671,0.015141511843));
#17383=CARTESIAN_POINT('',(-0.035223521483,0.009099035104,0.015362584279));
#17384=CARTESIAN_POINT('',(-0.035050225188,0.009108775673,0.01535752223));
#17385=CARTESIAN_POINT('',(-0.034963713862,0.009049994038,0.015218315908));
#17386=CARTESIAN_POINT('',(-0.035216913712,0.008964197582,0.015430279341));
#17387=CARTESIAN_POINT('',(-0.035043883179,0.008966030964,0.01542863008));
#17388=CARTESIAN_POINT('',(-0.034957106091,0.008895075333,0.015296202211));
#17389=CARTESIAN_POINT('',(-0.035223876434,0.00880361429,0.015533717464));
#17390=CARTESIAN_POINT('',(-0.035050518048,0.008797299153,0.015537902482));
#17391=CARTESIAN_POINT('',(-0.034964068813,0.008710470427,0.015414991225));
#17392=CARTESIAN_POINT('',(-0.03522604562,0.008771889308,0.015555375611));
#17393=CARTESIAN_POINT('',(-0.035052587043,0.008763972426,0.01556084085));
#17394=CARTESIAN_POINT('',(-0.034966237999,0.008673994043,0.015439854351));
#17395=CARTESIAN_POINT('',(-0.035231850552,0.008710185979,0.01559994762));
#17396=CARTESIAN_POINT('',(-0.035058120997,0.008699242413,0.015608106609));
#17397=CARTESIAN_POINT('',(-0.034972042931,0.008603038604,0.015491004502));
#17398=CARTESIAN_POINT('',(-0.0352354894,0.008680084706,0.015622937235));
#17399=CARTESIAN_POINT('',(-0.035061591095,0.00866769811700001,0.015632524608));
#17400=CARTESIAN_POINT('',(-0.034975681779,0.008568418251,0.01551737855));
#17401=CARTESIAN_POINT('',(-0.035248550352,0.008591972563,0.015693962252));
#17402=CARTESIAN_POINT('',(-0.035074046816,0.00857545401500001,0.015708073142));
#17403=CARTESIAN_POINT('',(-0.034988742731,0.008467061961,0.015598835312));
#17404=CARTESIAN_POINT('',(-0.035260111701,0.008536147393,0.015744048097));
#17405=CARTESIAN_POINT('',(-0.035085080525,0.008517189165,0.015761475243));
#17406=CARTESIAN_POINT('',(-0.03500030408,0.008402823979,0.015656246123));
#17407=CARTESIAN_POINT('',(-0.035281577861,0.008456663156,0.015823174106));
#17408=CARTESIAN_POINT('',(-0.035105505104,0.008434683838,0.015845779289));
#17409=CARTESIAN_POINT('',(-0.03502177024,0.00831133067,0.015746900341));
#17410=CARTESIAN_POINT('',(-0.035289421938,0.008430878868,0.015850217121));
#17411=CARTESIAN_POINT('',(-0.035112977015,0.008407947185,0.015874642529));
#17412=CARTESIAN_POINT('',(-0.035029614317,0.008281645265,0.015777876425));
#17413=CARTESIAN_POINT('',(-0.035306476701,0.008380728899,0.015905637862));
#17414=CARTESIAN_POINT('',(-0.035129211644,0.008356075565,0.015933800795));
#17415=CARTESIAN_POINT('',(-0.03504666908,0.008223896938,0.015841343859));
#17416=CARTESIAN_POINT('',(-0.035315718145,0.008356292952,0.015934104044));
#17417=CARTESIAN_POINT('',(-0.035138009535,0.008330862754,0.015964204293));
#17418=CARTESIAN_POINT('',(-0.035055910524,0.008195753062,0.015873936458));
#17419=CARTESIAN_POINT('',(-0.035345244257,0.008285697845,0.016020806527));
#17420=CARTESIAN_POINT('',(-0.035166136457,0.008258139049,0.01605692694));
#17421=CARTESIAN_POINT('',(-0.035085436637,0.008114429329,0.015973187908));
#17422=CARTESIAN_POINT('',(-0.035367258146,0.008242329816,0.016080187826));
#17423=CARTESIAN_POINT('',(-0.035187092355,0.00821380359800001,0.016120416082));
#17424=CARTESIAN_POINT('',(-0.035107450524,0.008064447951,0.016041138718));
#17425=CARTESIAN_POINT('',(-0.035415540032,0.008162463636,0.016201911227));
#17426=CARTESIAN_POINT('',(-0.035232955499,0.008132780528,0.016250421064));
#17427=CARTESIAN_POINT('',(-0.035155732411,0.007972359488,0.016180383385));
#17428=CARTESIAN_POINT('',(-0.035441809443,0.008125967618,0.016264254219));
#17429=CARTESIAN_POINT('',(-0.035257918294,0.008096097371,0.016317036983));
#17430=CARTESIAN_POINT('',(-0.035182001822,0.007930254845,0.016251678255));
#17431=CARTESIAN_POINT('',(-0.035498359317,0.008059587534,0.016391815963));
#17432=CARTESIAN_POINT('',(-0.035311533473,0.00803010615599999,0.016453125142));
#17433=CARTESIAN_POINT('',(-0.035238551696,0.007853625833,0.016397516267));
#17434=CARTESIAN_POINT('',(-0.035528803299,0.008029593217,0.016457359612));
#17435=CARTESIAN_POINT('',(-0.035340397738,0.008000717817,0.016523037284));
#17436=CARTESIAN_POINT('',(-0.035268995678,0.007818973813,0.016472430579));
#17437=CARTESIAN_POINT('',(-0.035624302868,0.007950706059,0.016654920378));
#17438=CARTESIAN_POINT('',(-0.035431143853,0.00792437715800001,0.016734311632));
#17439=CARTESIAN_POINT('',(-0.035364495247,0.007727753242,0.016698182027));
#17440=CARTESIAN_POINT('',(-0.035693625065,0.00791237942,0.016788320669));
#17441=CARTESIAN_POINT('',(-0.035496770299,0.007889702851,0.016876219964));
#17442=CARTESIAN_POINT('',(-0.035433817443,0.007683310981,0.016850547386));
#17443=CARTESIAN_POINT('',(-0.035804878296,0.007874305366,0.016990897542));
#17444=CARTESIAN_POINT('',(-0.035600812464,0.007858960081,0.01708919141));
#17445=CARTESIAN_POINT('',(-0.035545070675,0.0076389311,0.017081837817));
#17446=CARTESIAN_POINT('',(-0.035843360668,0.007864862098,0.01705913467));
#17447=CARTESIAN_POINT('',(-0.035636958249,0.007852300237,0.017161183879));
#17448=CARTESIAN_POINT('',(-0.035583553047,0.007627864561,0.017159732511));
#17449=CARTESIAN_POINT('',(-0.035921655233,0.007852607539,0.017194668761));
#17450=CARTESIAN_POINT('',(-0.035710302083,0.00784612017,0.017303741424));
#17451=CARTESIAN_POINT('',(-0.035661847612,0.007613348096,0.017314422362));
#17452=CARTESIAN_POINT('',(-0.035961464931,0.007849756022,0.017261981032));
#17453=CARTESIAN_POINT('',(-0.035747535996,0.007846637847,0.017374356859));
#17454=CARTESIAN_POINT('',(-0.035701657309,0.007609851942,0.017391235154));
#17455=CARTESIAN_POINT('',(-0.036082708725,0.007850536771,0.017462656398));
#17456=CARTESIAN_POINT('',(-0.035861344783,0.007858260977,0.017585519353));
#17457=CARTESIAN_POINT('',(-0.035822901104,0.007610083132,0.017620198615));
#17458=CARTESIAN_POINT('',(-0.036165937985,0.007863426326,0.017594770655));
#17459=CARTESIAN_POINT('',(-0.035938765603,0.00787975504900001,0.017722847129));
#17460=CARTESIAN_POINT('',(-0.035906130364,0.007624440672,0.017770889103));
#17461=CARTESIAN_POINT('',(-0.036272749616,0.007894708486,0.017757945878));
#17462=CARTESIAN_POINT('',(-0.036036325391,0.00792195592300001,0.017889160917));
#17463=CARTESIAN_POINT('',(-0.036012941995,0.007659800659,0.017956955579));
#17464=CARTESIAN_POINT('',(-0.036294271622,0.007901739857,0.017790509137));
#17465=CARTESIAN_POINT('',(-0.036056160144,0.007931321211,0.017922622722));
#17466=CARTESIAN_POINT('',(-0.036034464001,0.007667762066,0.017994084324));
#17467=CARTESIAN_POINT('',(-0.036337241164,0.007917210124,0.017854907701));
#17468=CARTESIAN_POINT('',(-0.036095695252,0.00795150851699999,0.01798864385));
#17469=CARTESIAN_POINT('',(-0.036077433543,0.007685302077,0.018067506581));
#17470=CARTESIAN_POINT('',(-0.036358730845,0.007925659835,0.017886808044));
#17471=CARTESIAN_POINT('',(-0.03611543566,0.00796235719799999,0.018021267296));
#17472=CARTESIAN_POINT('',(-0.036098923223,0.00769489288,0.018103874262));
#17473=CARTESIAN_POINT('',(-0.036423211553,0.007953112573,0.017981630573));
#17474=CARTESIAN_POINT('',(-0.036174782484,0.007997207555,0.018118355391));
#17475=CARTESIAN_POINT('',(-0.036163403931,0.00772608128,0.018211968175));
#17476=CARTESIAN_POINT('',(-0.036466213928,0.007974214849,0.018043676239));
#17477=CARTESIAN_POINT('',(-0.036214084658,0.008023322943,0.01818130788));
#17478=CARTESIAN_POINT('',(-0.036206406307,0.007750089872,0.018282687553));
#17479=CARTESIAN_POINT('',(-0.036595254777,0.008045769879,0.018226375241));
#17480=CARTESIAN_POINT('',(-0.03633245937,0.00811068502900001,0.018367068303));
#17481=CARTESIAN_POINT('',(-0.036335447156,0.007831586332,0.018490897658));
#17482=CARTESIAN_POINT('',(-0.036681322249,0.008104401696,0.018343621837));
#17483=CARTESIAN_POINT('',(-0.036410235723,0.00818013428299999,0.018483802691));
#17484=CARTESIAN_POINT('',(-0.036421514628,0.007898465521,0.018624476296));
#17485=CARTESIAN_POINT('',(-0.03678899075,0.008191880004,0.01848425171));
#17486=CARTESIAN_POINT('',(-0.036505370032,0.008279350682,0.018620167377));
#17487=CARTESIAN_POINT('',(-0.036529183129,0.007998347907,0.018784644787));
#17488=CARTESIAN_POINT('',(-0.036810556304,0.008210117449,0.01851211236));
#17489=CARTESIAN_POINT('',(-0.036524605066,0.00830017876799999,0.018647392468));
#17490=CARTESIAN_POINT('',(-0.036550748683,0.00801917556,0.018816373614));
#17491=CARTESIAN_POINT('',(-0.036853337272,0.008247729637,0.018566762019));
#17492=CARTESIAN_POINT('',(-0.036562661331,0.00834289234,0.018700571843));
#17493=CARTESIAN_POINT('',(-0.036593529651,0.008062137607,0.018878605442));
#17494=CARTESIAN_POINT('',(-0.036874593816,0.008267135902,0.018593605562));
#17495=CARTESIAN_POINT('',(-0.036581516731,0.008364823662,0.018726570453));
#17496=CARTESIAN_POINT('',(-0.036614786195,0.008084307983,0.018909170561));
#17497=CARTESIAN_POINT('',(-0.036937968442,0.00832714152,0.018672700842));
#17498=CARTESIAN_POINT('',(-0.03663781018,0.008432559434,0.018803151489));
#17499=CARTESIAN_POINT('',(-0.03667816082,0.008152871175,0.01899922333));
#17500=CARTESIAN_POINT('',(-0.03697969206,0.008369524049,0.018723520226));
#17501=CARTESIAN_POINT('',(-0.036674489896,0.00847979322399999,0.018851625693));
#17502=CARTESIAN_POINT('',(-0.036719884461,0.00820131189,0.019057071854));
#17503=CARTESIAN_POINT('',(-0.037020900622,0.008414292884,0.018772414733));
#17504=CARTESIAN_POINT('',(-0.036710197303,0.008528746736,0.01889741608));
#17505=CARTESIAN_POINT('',(-0.036761093001,0.008252492416,0.019112717618));
#17506=CARTESIAN_POINT('',(-0.0370209006225329,0.00819303142614902,0.0189750063603988));
#17507=CARTESIAN_POINT('',(-0.036382929700134,0.0117699983702051,0.0156265169988629));
#17508=CARTESIAN_POINT('',(-0.0370209006725265,0.00841429293889186,0.0187724147929504));
#17509=CARTESIAN_POINT('',(-0.0367101973471479,0.00852874679652508,0.0188974161366142));
#17510=CARTESIAN_POINT('',(-0.0367610930515268,0.00825249247875368,0.0191127176862286));
#17511=CARTESIAN_POINT('',(-0.037103317012847,0.00850382975946811,0.0188702028728446));
#17512=CARTESIAN_POINT('',(-0.0367834353017993,0.00862915328424696,0.0189913348642332));
#17513=CARTESIAN_POINT('',(-0.0368435097848469,0.00835485310428282,0.0192240087409122));
#17514=CARTESIAN_POINT('',(-0.0371836845969985,0.00860284405433526,0.018960351265708));
#17515=CARTESIAN_POINT('',(-0.036852619292111,0.00873678178590861,0.0190740421504255));
#17516=CARTESIAN_POINT('',(-0.0369238769759985,0.0084680943925531,0.0193265564529946));
#17517=CARTESIAN_POINT('',(-0.037301116085,0.008766788714,0.019082991418));
#17518=CARTESIAN_POINT('',(-0.03695137278,0.00890933196,0.019182696761));
#17519=CARTESIAN_POINT('',(-0.037041308464,0.008655658553,0.019465980183));
#17520=CARTESIAN_POINT('',(-0.037339424126,0.008823609321,0.019121421839));
#17521=CARTESIAN_POINT('',(-0.036983551057,0.008969082356,0.019216348303));
#17522=CARTESIAN_POINT('',(-0.037079616505,0.008720674816,0.019509653949));
#17523=CARTESIAN_POINT('',(-0.037413681214,0.008940547851,0.01919260491));
#17524=CARTESIAN_POINT('',(-0.037045412802,0.009090762045,0.019277559802));
#17525=CARTESIAN_POINT('',(-0.037153873593,0.00885449785,0.019590514456));
#17526=CARTESIAN_POINT('',(-0.037449744946,0.00900082422,0.019225478294));
#17527=CARTESIAN_POINT('',(-0.037075133644,0.00915286487800001,0.019305105559));
#17528=CARTESIAN_POINT('',(-0.037189937325,0.008923485888,0.019627838465));
#17529=CARTESIAN_POINT('',(-0.037519742735,0.009125063699,0.01928564172));
#17530=CARTESIAN_POINT('',(-0.0371322980209999,0.009279487072,0.019354318908));
#17531=CARTESIAN_POINT('',(-0.037259935114,0.009065697806,0.019696105522));
#17532=CARTESIAN_POINT('',(-0.037553677068,0.009189026182,0.019312932788));
#17533=CARTESIAN_POINT('',(-0.037159681014,0.009344000008,0.019375867489));
#17534=CARTESIAN_POINT('',(-0.037293869447,0.009138920963,0.019727049749));
#17535=CARTESIAN_POINT('',(-0.037602938649,0.009287868388,0.019349449243));
#17536=CARTESIAN_POINT('',(-0.037198872381,0.009442158226,0.01940357468));
#17537=CARTESIAN_POINT('',(-0.037343131027,0.009252085639,0.019768414058));
#17538=CARTESIAN_POINT('',(-0.037619085386,0.009321299752,0.01936088333));
#17539=CARTESIAN_POINT('',(-0.037211691522,0.00947530986300001,0.0194120754));
#17540=CARTESIAN_POINT('',(-0.037359277765,0.009290363203,0.019781358588));
#17541=CARTESIAN_POINT('',(-0.037650817756,0.009389164887,0.019382217481));
#17542=CARTESIAN_POINT('',(-0.037236742776,0.00954221984800001,0.019427532009));
#17543=CARTESIAN_POINT('',(-0.037391010135,0.00936806994,0.019805494239));
#17544=CARTESIAN_POINT('',(-0.037666411882,0.009423626067,0.019392118348));
#17545=CARTESIAN_POINT('',(-0.037248972401,0.00957599822699999,0.019434471815));
#17546=CARTESIAN_POINT('',(-0.037406604261,0.009407530512,0.019816686195));
#17547=CARTESIAN_POINT('',(-0.037742059103,0.009596469576,0.019437127945));
#17548=CARTESIAN_POINT('',(-0.037308672836,0.009746481892,0.019465277981));
#17549=CARTESIAN_POINT('',(-0.037482251481,0.009605458605,0.0198675155));
#17550=CARTESIAN_POINT('',(-0.037795953594,0.009737990873,0.019459408654));
#17551=CARTESIAN_POINT('',(-0.037349209561,0.00988085362500001,0.019475955808));
#17552=CARTESIAN_POINT('',(-0.037536145973,0.009767548722,0.019892505579));
#17553=CARTESIAN_POINT('',(-0.037866774638,0.00995526822,0.019471266124));
#17554=CARTESIAN_POINT('',(-0.037401307565,0.010081722694,0.019473703662));
#17555=CARTESIAN_POINT('',(-0.037606967016,0.010016452968,0.019905364135));
#17556=CARTESIAN_POINT('',(-0.037888699602,0.010028532389,0.019471600233));
#17557=CARTESIAN_POINT('',(-0.037417279271,0.010149079247,0.019469741824));
#17558=CARTESIAN_POINT('',(-0.037628891981,0.010100389312,0.019905517967));
#17559=CARTESIAN_POINT('',(-0.037918925522,0.010139765166,0.0194662815));
#17560=CARTESIAN_POINT('',(-0.037439020962,0.010250061616,0.019459037412));
#17561=CARTESIAN_POINT('',(-0.037659117901,0.010227838031,0.01989910134));
#17562=CARTESIAN_POINT('',(-0.037928582819,0.010177183975,0.019463520333));
#17563=CARTESIAN_POINT('',(-0.037445936687,0.010283943964,0.019454625919));
#17564=CARTESIAN_POINT('',(-0.037668775198,0.010270714068,0.019895833342));
#17565=CARTESIAN_POINT('',(-0.037946745879,0.010251529703,0.019456070883));
#17566=CARTESIAN_POINT('',(-0.037458875717,0.010350958591,0.019444295419));
#17567=CARTESIAN_POINT('',(-0.037686938258,0.01035590701,0.019887098991));
#17568=CARTESIAN_POINT('',(-0.03795527555,0.010288532493,0.019451385246));
#17569=CARTESIAN_POINT('',(-0.0374649083939999,0.010384139251,0.019438369006));
#17570=CARTESIAN_POINT('',(-0.037695467929,0.010398310834,0.019881635422));
#17571=CARTESIAN_POINT('',(-0.037995201404,0.0104727007,0.019423189771));
#17572=CARTESIAN_POINT('',(-0.037493219634,0.010549838583,0.019404818528));
#17573=CARTESIAN_POINT('',(-0.037735393783,0.010609372239,0.01984887779));
#17574=CARTESIAN_POINT('',(-0.03801852767,0.010617356474,0.019385538099));
#17575=CARTESIAN_POINT('',(-0.0375089769519999,0.010676036879,0.019366609516));
#17576=CARTESIAN_POINT('',(-0.037758720049,0.010775187757,0.01980544701));
#17577=CARTESIAN_POINT('',(-0.038040144091,0.010830087113,0.019305249844));
#17578=CARTESIAN_POINT('',(-0.037523624808,0.010861368197,0.019291823728));
#17579=CARTESIAN_POINT('',(-0.03778033647,0.011019102134,0.019713124546));
#17580=CARTESIAN_POINT('',(-0.038045091154,0.010900659463,0.01927424932));
#17581=CARTESIAN_POINT('',(-0.037526947936,0.010922751921,0.019263695619));
#17582=CARTESIAN_POINT('',(-0.037785283533,0.011100031176,0.01967751236));
#17583=CARTESIAN_POINT('',(-0.038050108278,0.011036551943,0.019205674484));
#17584=CARTESIAN_POINT('',(-0.037530327064,0.011041355675,0.019202654737));
#17585=CARTESIAN_POINT('',(-0.037790300657,0.011255891492,0.01959879628));
#17586=CARTESIAN_POINT('',(-0.038050243047,0.011102269591,0.019167998017));
#17587=CARTESIAN_POINT('',(-0.037530417095,0.011098746343,0.01916971836));
#17588=CARTESIAN_POINT('',(-0.037790435426,0.011331278423,0.019555574534));
#17589=CARTESIAN_POINT('',(-0.038045857381,0.011229333988,0.019085998172));
#17590=CARTESIAN_POINT('',(-0.037527464034,0.011210579299,0.019098653928));
#17591=CARTESIAN_POINT('',(-0.03778604976,0.011477065914,0.019461552266));
#17592=CARTESIAN_POINT('',(-0.038041336883,0.011290680666,0.019041674687));
#17593=CARTESIAN_POINT('',(-0.037524429559,0.011264860653,0.019060637682));
#17594=CARTESIAN_POINT('',(-0.037781529262,0.011547466388,0.019410751623));
#17595=CARTESIAN_POINT('',(-0.038027559938,0.011408940944,0.018946286813));
#17596=CARTESIAN_POINT('',(-0.037515080889,0.011370775304,0.018978926179));
#17597=CARTESIAN_POINT('',(-0.037767752317,0.011683211699,0.019301463566));
#17598=CARTESIAN_POINT('',(-0.038018235775,0.011465994202,0.018895009009));
#17599=CARTESIAN_POINT('',(-0.037508746133,0.011422411288,0.018935184096));
#17600=CARTESIAN_POINT('',(-0.037758428154,0.011748717175,0.019242731993));
#17601=CARTESIAN_POINT('',(-0.037983863425,0.011626135813,0.018735057854));
#17602=CARTESIAN_POINT('',(-0.037485152239,0.011569149469,0.018798617961));
#17603=CARTESIAN_POINT('',(-0.037724055805,0.011932636702,0.01905958005));
#17604=CARTESIAN_POINT('',(-0.03795238138,0.011719875549,0.018619223276));
#17605=CARTESIAN_POINT('',(-0.037463427014,0.011658126499,0.018699531784));
#17606=CARTESIAN_POINT('',(-0.037692573758,0.012040369285,0.018927005758));
#17607=CARTESIAN_POINT('',(-0.037902538675,0.01182142833,0.018463435089));
#17608=CARTESIAN_POINT('',(-0.037427207905,0.011759803085,0.018561524169));
#17609=CARTESIAN_POINT('',(-0.037642731053,0.012157190014,0.018748770563));
#17610=CARTESIAN_POINT('',(-0.0378920119,0.011840990207,0.018431644379));
#17611=CARTESIAN_POINT('',(-0.037419583631,0.011779451696,0.018533495969));
#17612=CARTESIAN_POINT('',(-0.037632204279,0.012179699312,0.018712402395));
#17613=CARTESIAN_POINT('',(-0.037870126119,0.011878130234,0.018367644958));
#17614=CARTESIAN_POINT('',(-0.037403612981,0.011817220648,0.018476768706));
#17615=CARTESIAN_POINT('',(-0.037610318498,0.012222448524,0.018639193956));
#17616=CARTESIAN_POINT('',(-0.037858748966,0.011895754219,0.018335374301));
#17617=CARTESIAN_POINT('',(-0.037395262434,0.011835384713,0.018448035028));
#17618=CARTESIAN_POINT('',(-0.037598941345,0.012242741131,0.018602282796));
#17619=CARTESIAN_POINT('',(-0.037823348421,0.011945883489,0.018237779846));
#17620=CARTESIAN_POINT('',(-0.037369172913,0.011887572482,0.018360946022));
#17621=CARTESIAN_POINT('',(-0.0375635408,0.012300482293,0.018490662919));
#17622=CARTESIAN_POINT('',(-0.037798059306,0.011975653238,0.018171675593));
#17623=CARTESIAN_POINT('',(-0.037350277137,0.011919662954,0.018301226609));
#17624=CARTESIAN_POINT('',(-0.037538251684,0.012334802364,0.01841507009));
#17625=CARTESIAN_POINT('',(-0.037744193093,0.012028207852,0.018037491178));
#17626=CARTESIAN_POINT('',(-0.037309379895,0.011978153369,0.018178502137));
#17627=CARTESIAN_POINT('',(-0.037484385472,0.012395455267,0.018261646389));
#17628=CARTESIAN_POINT('',(-0.037715615604,0.012050991651,0.017969410681));
#17629=CARTESIAN_POINT('',(-0.037287455068,0.012004589867,0.018115639729));
#17630=CARTESIAN_POINT('',(-0.037455807983,0.012421786873,0.018183815137));
#17631=CARTESIAN_POINT('',(-0.037670271841,0.012079999243,0.017865841447));
#17632=CARTESIAN_POINT('',(-0.037251993154,0.012039949422,0.018018443323));
#17633=CARTESIAN_POINT('',(-0.03741046422,0.012455375111,0.018065427979));
#17634=CARTESIAN_POINT('',(-0.037654725402,0.012088808864,0.017831040227));
#17635=CARTESIAN_POINT('',(-0.037239813053,0.012050965676,0.017985742729));
#17636=CARTESIAN_POINT('',(-0.037394917781,0.012465588496,0.018025650255));
#17637=CARTESIAN_POINT('',(-0.037623119912,0.012104555629,0.017761655615));
#17638=CARTESIAN_POINT('',(-0.037214887215,0.012071290256,0.017920179797));
#17639=CARTESIAN_POINT('',(-0.037363312291,0.012483871576,0.017946348883));
#17640=CARTESIAN_POINT('',(-0.037607024828,0.012111518654,0.017726988147));
#17641=CARTESIAN_POINT('',(-0.037202122033,0.012080639592,0.017887250964));
#17642=CARTESIAN_POINT('',(-0.037347217206,0.012491971204,0.017906729123));
#17643=CARTESIAN_POINT('',(-0.037525118351,0.012141933343,0.01755377779));
#17644=CARTESIAN_POINT('',(-0.037137549676,0.012122798947,0.017723852461));
#17645=CARTESIAN_POINT('',(-0.03726531073,0.012527433166,0.017708787883));
#17646=CARTESIAN_POINT('',(-0.037455051799,0.012152306816,0.017415613082));
#17647=CARTESIAN_POINT('',(-0.037080651573,0.012144510573,0.017589399015));
#17648=CARTESIAN_POINT('',(-0.037195244178,0.012539827994,0.017550935495));
#17649=CARTESIAN_POINT('',(-0.037343235527,0.012148213531,0.01720905843));
#17650=CARTESIAN_POINT('',(-0.036986748025,0.012157127057,0.017382507888));
#17651=CARTESIAN_POINT('',(-0.037083427906,0.012535928527,0.017315007876));
#17652=CARTESIAN_POINT('',(-0.03730475018,0.012143504287,0.01714019209));
#17653=CARTESIAN_POINT('',(-0.03695443279,0.012158057656,0.017313516891));
#17654=CARTESIAN_POINT('',(-0.037044942559,0.012530801323,0.017236358679));
#17655=CARTESIAN_POINT('',(-0.03722687049,0.012127824497,0.017005091856));
#17656=CARTESIAN_POINT('',(-0.036888415857,0.012153246959,0.017177025003));
#17657=CARTESIAN_POINT('',(-0.036967062869,0.012513372076,0.01708208731));
#17658=CARTESIAN_POINT('',(-0.037187320072,0.012116862461,0.016938559819));
#17659=CARTESIAN_POINT('',(-0.036854627768,0.012147650578,0.017109245591));
#17660=CARTESIAN_POINT('',(-0.036927512451,0.012501080898,0.017006124553));
#17661=CARTESIAN_POINT('',(-0.03706685504,0.012075016713,0.016741914748));
#17662=CARTESIAN_POINT('',(-0.036751742399,0.012121386905,0.016909119768));
#17663=CARTESIAN_POINT('',(-0.036807047419,0.012453943078,0.016781637365));
#17664=CARTESIAN_POINT('',(-0.03698413842,0.012035245207,0.016614730411));
#17665=CARTESIAN_POINT('',(-0.036679594089,0.012091526511,0.016776553485));
#17666=CARTESIAN_POINT('',(-0.036724330798,0.01240891457,0.016636488213));
#17667=CARTESIAN_POINT('',(-0.036813690053,0.011932224721,0.016368219888));
#17668=CARTESIAN_POINT('',(-0.036528822624,0.012005165032,0.016516491866));
#17669=CARTESIAN_POINT('',(-0.036553882432,0.012291955726,0.016355253995));
#17670=CARTESIAN_POINT('',(-0.03672806298,0.011870246798,0.016251941319));
#17671=CARTESIAN_POINT('',(-0.036452219097,0.011950532581,0.016391983009));
#17672=CARTESIAN_POINT('',(-0.036468255359,0.012221468356,0.016222645908));
#17673=CARTESIAN_POINT('',(-0.036556082968,0.011726690875,0.01603279824));
#17674=CARTESIAN_POINT('',(-0.036296957641,0.01181811194,0.016155409747));
#17675=CARTESIAN_POINT('',(-0.036296275347,0.012057999557,0.015972835599));
#17676=CARTESIAN_POINT('',(-0.036469700557,0.011645092454,0.01592989329));
#17677=CARTESIAN_POINT('',(-0.036218299035,0.011740996991,0.016042857153));
#17678=CARTESIAN_POINT('',(-0.03620989256,0.011964994531,0.015855586742));
#17679=CARTESIAN_POINT('',(-0.0363829297,0.011553263876,0.015833944478));
#17680=CARTESIAN_POINT('',(-0.036137554584,0.011650536133,0.015935581221));
#17681=CARTESIAN_POINT('',(-0.036123122079,0.011860244082,0.015746332321));
#17682=CARTESIAN_POINT('',(-0.0387712812904556,1.29145419960524E-11,1.90093214813058E-11));
#17683=CARTESIAN_POINT('',(-0.0363829297,-0.007935966222,0.017922392252));
#17684=CARTESIAN_POINT('',(-0.036137554584,-0.00797535009500001,0.01805745087));
#17685=CARTESIAN_POINT('',(-0.036123122079,-0.007706601765,0.018144438831));
#17686=CARTESIAN_POINT('',(-0.036296388628,-0.00789888486,0.017795229609));
#17687=CARTESIAN_POINT('',(-0.036059352191,-0.00792917773300001,0.017929626577));
#17688=CARTESIAN_POINT('',(-0.03603658062,-0.007664471384,0.017999478691));
#17689=CARTESIAN_POINT('',(-0.036211750879,-0.007873865053,0.017666078425));
#17690=CARTESIAN_POINT('',(-0.03598108599,-0.007894696976,0.017796520282));
#17691=CARTESIAN_POINT('',(-0.035951943258,-0.00763618434,0.017852211978));
#17692=CARTESIAN_POINT('',(-0.036046427611,-0.007847575992,0.017403812149));
#17693=CARTESIAN_POINT('',(-0.03582764111,-0.007852090759,0.01752422126));
#17694=CARTESIAN_POINT('',(-0.03578661999,-0.007606880233,0.017553069188));
#17695=CARTESIAN_POINT('',(-0.035965731891,-0.007846286179,0.017270695297));
#17696=CARTESIAN_POINT('',(-0.035752240428,-0.007843210526,0.017384956612));
#17697=CARTESIAN_POINT('',(-0.03570592427,-0.00760583974,0.017401191901));
#17698=CARTESIAN_POINT('',(-0.035867783855,-0.007860916809,0.017101471238));
#17699=CARTESIAN_POINT('',(-0.035659677357,-0.00785025534,0.017205405462));
#17700=CARTESIAN_POINT('',(-0.035607976234,-0.007623195358,0.017208053208));
#17701=CARTESIAN_POINT('',(-0.03584830488,-0.007864675489,0.017067415562));
#17702=CARTESIAN_POINT('',(-0.035641412325,-0.00785254753800001,0.017169542439));
#17703=CARTESIAN_POINT('',(-0.035588497259,-0.007627622941,0.017169181517));
#17704=CARTESIAN_POINT('',(-0.035810061793,-0.007873792339,0.016999715979));
#17705=CARTESIAN_POINT('',(-0.035605524332,-0.007858918629,0.017098165957));
#17706=CARTESIAN_POINT('',(-0.035550254172,-0.007638313039,0.017091901304));
#17707=CARTESIAN_POINT('',(-0.035791254693,-0.00787915358,0.016965999395));
#17708=CARTESIAN_POINT('',(-0.035587855191,-0.00786298741,0.01706256955));
#17709=CARTESIAN_POINT('',(-0.035531447072,-0.007644579318,0.017053409847));
#17710=CARTESIAN_POINT('',(-0.035735788251,-0.007897644484,0.016865244352));
#17711=CARTESIAN_POINT('',(-0.035535852231,-0.00787783087500001,0.016956380478));
#17712=CARTESIAN_POINT('',(-0.03547598063,-0.007666140505,0.016938375535));
#17713=CARTESIAN_POINT('',(-0.035700081089,-0.007913175312,0.016798599729));
#17714=CARTESIAN_POINT('',(-0.035502196601,-0.007891267476,0.016885756544));
#17715=CARTESIAN_POINT('',(-0.035440273468,-0.007684190871,0.016862271769));
#17716=CARTESIAN_POINT('',(-0.035596955729,-0.007969579454,0.016600233953));
#17717=CARTESIAN_POINT('',(-0.035405412743,-0.007942282341,0.016676313757));
#17718=CARTESIAN_POINT('',(-0.035337148108,-0.007749601706,0.016635705408));
#17719=CARTESIAN_POINT('',(-0.035533471872,-0.008020130655,0.016470062373));
#17720=CARTESIAN_POINT('',(-0.03534514464,-0.007990615333,0.016537412932));
#17721=CARTESIAN_POINT('',(-0.035273664252,-0.00780806873,0.016486967212));
#17722=CARTESIAN_POINT('',(-0.035462076716,-0.008101852446,0.016310148785));
#17723=CARTESIAN_POINT('',(-0.035277056499,-0.008072198153,0.016365801681));
#17724=CARTESIAN_POINT('',(-0.035202269094,-0.007902417857,0.016304149447));
#17725=CARTESIAN_POINT('',(-0.035448157312,-0.008119195502,0.016278204166));
#17726=CARTESIAN_POINT('',(-0.035263851039,-0.00808951015200001,0.016331706315));
#17727=CARTESIAN_POINT('',(-0.035188349691,-0.007922433981,0.016267624501));
#17728=CARTESIAN_POINT('',(-0.035421421576,-0.008155528492,0.01621518104));
#17729=CARTESIAN_POINT('',(-0.035238481118,-0.008125981757,0.0162644302));
#17730=CARTESIAN_POINT('',(-0.035161613954,-0.007964353608,0.016195554481));
#17731=CARTESIAN_POINT('',(-0.035408615027,-0.008174492909,0.016184132248));
#17732=CARTESIAN_POINT('',(-0.035226318844,-0.008145113188,0.016231268977));
#17733=CARTESIAN_POINT('',(-0.035148807406,-0.007986227718,0.01616004343));
#17734=CARTESIAN_POINT('',(-0.035371903227,-0.008233790533,0.016092375852));
#17735=CARTESIAN_POINT('',(-0.035191509303,-0.008205098964,0.016133439925));
#17736=CARTESIAN_POINT('',(-0.035112095605,-0.008054604749,0.016055083828));
#17737=CARTESIAN_POINT('',(-0.035349701075,-0.00827652121,0.01603305419));
#17738=CARTESIAN_POINT('',(-0.035170375015,-0.008248745904,0.016070010593));
#17739=CARTESIAN_POINT('',(-0.035089893455,-0.008103854486,0.015987204245));
#17740=CARTESIAN_POINT('',(-0.035310076825,-0.008368595603,0.015918211266));
#17741=CARTESIAN_POINT('',(-0.035132682741,-0.008343387593,0.015947352599));
#17742=CARTESIAN_POINT('',(-0.035050269204,-0.008209928279,0.015855746634));
#17743=CARTESIAN_POINT('',(-0.035292653375,-0.008417937511,0.015862688976));
#17744=CARTESIAN_POINT('',(-0.035116074086,-0.008394403586,0.015888019139));
#17745=CARTESIAN_POINT('',(-0.035032845755,-0.008266750265,0.015792167434));
#17746=CARTESIAN_POINT('',(-0.035270404132,-0.008497251596,0.015782437272));
#17747=CARTESIAN_POINT('',(-0.035094864144,-0.00847684110199999,0.015802332322));
#17748=CARTESIAN_POINT('',(-0.03501059651,-0.00835805282,0.015700230057));
#17749=CARTESIAN_POINT('',(-0.03526362249,-0.008524662259,0.015756120857));
#17750=CARTESIAN_POINT('',(-0.035088401673,-0.008505365652,0.015774270534));
#17751=CARTESIAN_POINT('',(-0.035003814869,-0.008389601082,0.015670074582));
#17752=CARTESIAN_POINT('',(-0.035251577427,-0.008580564888,0.015705227052));
#17753=CARTESIAN_POINT('',(-0.035076925826,-0.008563640037,0.01572005437));
#17754=CARTESIAN_POINT('',(-0.034991769806,-0.008453930794,0.015611741863));
#17755=CARTESIAN_POINT('',(-0.035246291308,-0.008609118788,0.015680578683));
#17756=CARTESIAN_POINT('',(-0.035071886429,-0.008593462603,0.015693811186));
#17757=CARTESIAN_POINT('',(-0.034986483687,-0.008486783572,0.015583483346));
#17758=CARTESIAN_POINT('',(-0.035223521483,-0.008754870702,0.01556128769));
#17759=CARTESIAN_POINT('',(-0.035050225188,-0.008745616554,0.015567192245));
#17760=CARTESIAN_POINT('',(-0.034963713862,-0.008654451161,0.015446682695));
#17761=CARTESIAN_POINT('',(-0.035216913712,-0.008880915106,0.0154783625));
#17762=CARTESIAN_POINT('',(-0.035043883179,-0.008878570113,0.015479125626));
#17763=CARTESIAN_POINT('',(-0.034957106091,-0.00879936203,0.015351462313));
#17764=CARTESIAN_POINT('',(-0.035223876434,-0.009050786794,0.015391012352));
#17765=CARTESIAN_POINT('',(-0.035050518048,-0.00905756869499999,0.015387635792));
#17766=CARTESIAN_POINT('',(-0.034964068813,-0.008994538787,0.015250984281));
#17767=CARTESIAN_POINT('',(-0.03522604562,-0.00908540579,0.015374366785));
#17768=CARTESIAN_POINT('',(-0.035052587043,-0.009094097267,0.015370243184));
#17769=CARTESIAN_POINT('',(-0.034966237999,-0.009034309077,0.015231826369));
#17770=CARTESIAN_POINT('',(-0.035231850552,-0.009154857947,0.015343216139));
#17771=CARTESIAN_POINT('',(-0.035058120997,-0.00916739562200001,0.015337818228));
#17772=CARTESIAN_POINT('',(-0.034972042931,-0.009114084127,0.015195952232));
#17773=CARTESIAN_POINT('',(-0.0352354894,-0.009189818174,0.015328642479));
#17774=CARTESIAN_POINT('',(-0.035061591095,-0.009204314377,0.015322709066));
#17775=CARTESIAN_POINT('',(-0.034975681779,-0.009154234899,0.01517915715));
#17776=CARTESIAN_POINT('',(-0.035248550352,-0.009295383715,0.015287847634));
#17777=CARTESIAN_POINT('',(-0.035074046816,-0.00931586337799999,0.015280597597));
#17778=CARTESIAN_POINT('',(-0.034988742731,-0.009275456669,0.01513210841));
#17779=CARTESIAN_POINT('',(-0.035260111701,-0.009366671914,0.015264544541));
#17780=CARTESIAN_POINT('',(-0.035085080525,-0.009391243379,0.015256839807));
#17781=CARTESIAN_POINT('',(-0.03500030408,-0.009357294881,0.01510518209));
#17782=CARTESIAN_POINT('',(-0.035281577861,-0.009474939166,0.015235272178));
#17783=CARTESIAN_POINT('',(-0.035105505104,-0.00950550548799999,0.015227540121));
#17784=CARTESIAN_POINT('',(-0.03502177024,-0.009481550391,0.01507127367));
#17785=CARTESIAN_POINT('',(-0.035289421938,-0.009511251248,0.015226463836));
#17786=CARTESIAN_POINT('',(-0.035112977015,-0.00954387011300001,0.01521881712));
#17787=CARTESIAN_POINT('',(-0.035029614317,-0.009523219169,0.015061053398));
#17788=CARTESIAN_POINT('',(-0.035306476701,-0.009584322003,0.01521074306));
#17789=CARTESIAN_POINT('',(-0.035129211644,-0.009621038485,0.015203474112));
#17790=CARTESIAN_POINT('',(-0.03504666908,-0.009607057743,0.015042775596));
#17791=CARTESIAN_POINT('',(-0.035315718145,-0.009621192412,0.015203814));
#17792=CARTESIAN_POINT('',(-0.035138009535,-0.009659975092,0.015196840927));
#17793=CARTESIAN_POINT('',(-0.035055910524,-0.0096493557,0.015034698584));
#17794=CARTESIAN_POINT('',(-0.035345244257,-0.009731576519,0.015186028085));
#17795=CARTESIAN_POINT('',(-0.035166136457,-0.009776637113,0.015180221674));
#17796=CARTESIAN_POINT('',(-0.035085436637,-0.009775971844,0.01501389589));
#17797=CARTESIAN_POINT('',(-0.035367258146,-0.009804686247,0.01517816092));
#17798=CARTESIAN_POINT('',(-0.035187092355,-0.00985378804700001,0.015173570618));
#17799=CARTESIAN_POINT('',(-0.035107450524,-0.009859809659,0.015004586152));
#17800=CARTESIAN_POINT('',(-0.035415540032,-0.009950034894,0.01516985648));
#17801=CARTESIAN_POINT('',(-0.035232955499,-0.010006887199,0.015168405072));
#17802=CARTESIAN_POINT('',(-0.035155732411,-0.01002644331,0.014994457537));
#17803=CARTESIAN_POINT('',(-0.035441809443,-0.010022273518,0.015169421497));
#17804=CARTESIAN_POINT('',(-0.035257918294,-0.010082919856,0.015169944486));
#17805=CARTESIAN_POINT('',(-0.035182001822,-0.0101092388,0.014993641282));
#17806=CARTESIAN_POINT('',(-0.035498359317,-0.010165935271,0.01517571553));
#17807=CARTESIAN_POINT('',(-0.035311533473,-0.010233771266,0.015180838497));
#17808=CARTESIAN_POINT('',(-0.035238551696,-0.01027385273,0.015000197616));
#17809=CARTESIAN_POINT('',(-0.035528803299,-0.010237694895,0.015182511514));
#17810=CARTESIAN_POINT('',(-0.035340397738,-0.010309011127,0.01519034352));
#17811=CARTESIAN_POINT('',(-0.035268995678,-0.010356056437,0.015007645243));
#17812=CARTESIAN_POINT('',(-0.035624302868,-0.010448231116,0.015212973614));
#17813=CARTESIAN_POINT('',(-0.035431143853,-0.010530150409,0.015229867744));
#17814=CARTESIAN_POINT('',(-0.035364495247,-0.010597173211,0.015041521636));
#17815=CARTESIAN_POINT('',(-0.035693625065,-0.010582922476,0.015246481917));
#17816=CARTESIAN_POINT('',(-0.035496770299,-0.010670383783,0.015270793079));
#17817=CARTESIAN_POINT('',(-0.035433817443,-0.010751346613,0.015079216188));
#17818=CARTESIAN_POINT('',(-0.035804878296,-0.010777396222,0.015314797255));
#17819=CARTESIAN_POINT('',(-0.035600812464,-0.010870193851,0.015350654782));
#17820=CARTESIAN_POINT('',(-0.035545070675,-0.010973839943,0.015156427299));
#17821=CARTESIAN_POINT('',(-0.035843360668,-0.010841212942,0.01534073771));
#17822=CARTESIAN_POINT('',(-0.035636958249,-0.01093587108,0.015380883423));
#17823=CARTESIAN_POINT('',(-0.035583553047,-0.011046831996,0.015185790742));
#17824=CARTESIAN_POINT('',(-0.035921655233,-0.010964716188,0.015397891995));
#17825=CARTESIAN_POINT('',(-0.035710302083,-0.011062419569,0.015446810101));
#17826=CARTESIAN_POINT('',(-0.035661847612,-0.011188055569,0.01525056404));
#17827=CARTESIAN_POINT('',(-0.035961464931,-0.011024436082,0.015429078645));
#17828=CARTESIAN_POINT('',(-0.035747535996,-0.011123315491,0.015482566139));
#17829=CARTESIAN_POINT('',(-0.035701657309,-0.011256325476,0.015285942678));
#17830=CARTESIAN_POINT('',(-0.036082708725,-0.011197835672,0.015530092476));
#17831=CARTESIAN_POINT('',(-0.035861344783,-0.01130037601,0.015598213312));
#17832=CARTESIAN_POINT('',(-0.035822901104,-0.011454498054,0.015400624625));
#17833=CARTESIAN_POINT('',(-0.036165937985,-0.011305805198,0.015607312287));
#17834=CARTESIAN_POINT('',(-0.035938765603,-0.011408558316,0.015685491612));
#17835=CARTESIAN_POINT('',(-0.035906130364,-0.011577821075,0.015488403863));
#17836=CARTESIAN_POINT('',(-0.036272749616,-0.011431478006,0.015715991043));
#17837=CARTESIAN_POINT('',(-0.036036325391,-0.011531489845,0.015805195535));
#17838=CARTESIAN_POINT('',(-0.036012941995,-0.011721279377,0.015612059748));
#17839=CARTESIAN_POINT('',(-0.036294271622,-0.011456162931,0.015738362019));
#17840=CARTESIAN_POINT('',(-0.036056160144,-0.011555785974,0.015830037016));
#17841=CARTESIAN_POINT('',(-0.036034464001,-0.011749453109,0.015637518901));
#17842=CARTESIAN_POINT('',(-0.036337241164,-0.011504198589,0.015783958945));
#17843=CARTESIAN_POINT('',(-0.036095695252,-0.011602868295,0.015880530299));
#17844=CARTESIAN_POINT('',(-0.036077433543,-0.011804268644,0.015689420125));
#17845=CARTESIAN_POINT('',(-0.036358730845,-0.011527600241,0.015807226781));
#17846=CARTESIAN_POINT('',(-0.03611543566,-0.011625696687,0.015906237255));
#17847=CARTESIAN_POINT('',(-0.036098923223,-0.011830968578,0.015715909844));
#17848=CARTESIAN_POINT('',(-0.036423211553,-0.011595992591,0.015878412814));
#17849=CARTESIAN_POINT('',(-0.036174782484,-0.011692352266,0.015984962597));
#17850=CARTESIAN_POINT('',(-0.036163403931,-0.011908986452,0.015796966748));
#17851=CARTESIAN_POINT('',(-0.036466213928,-0.011639174576,0.015927710753));
#17852=CARTESIAN_POINT('',(-0.036214084658,-0.011733813027,0.016039055431));
#17853=CARTESIAN_POINT('',(-0.036206406307,-0.011958226934,0.015853118487));
#17854=CARTESIAN_POINT('',(-0.036595254777,-0.011761619038,0.016081028728));
#17855=CARTESIAN_POINT('',(-0.03633245937,-0.011851005228,0.016207593429));
#17856=CARTESIAN_POINT('',(-0.036335447156,-0.012097793945,0.016027801545));
#17857=CARTESIAN_POINT('',(-0.036681322249,-0.01183384166,0.01619042867));
#17858=CARTESIAN_POINT('',(-0.036410235723,-0.011917375548,0.016326105441));
#17859=CARTESIAN_POINT('',(-0.036421514628,-0.012180036844,0.016152509941));
#17860=CARTESIAN_POINT('',(-0.03678899075,-0.011911891549,0.016336502043));
#17861=CARTESIAN_POINT('',(-0.036505370032,-0.01198586263,0.016480211706));
#17862=CARTESIAN_POINT('',(-0.036529183129,-0.012268805633,0.016319094869));
#17863=CARTESIAN_POINT('',(-0.036810556304,-0.011926900857,0.016366226459));
#17864=CARTESIAN_POINT('',(-0.036524605066,-0.011999026208,0.016511861903));
#17865=CARTESIAN_POINT('',(-0.036550748683,-0.012285869776,0.016352996559));
#17866=CARTESIAN_POINT('',(-0.036853337272,-0.011955422756,0.016426124399));
#17867=CARTESIAN_POINT('',(-0.036562661331,-0.012023724111,0.016575442629));
#17868=CARTESIAN_POINT('',(-0.036593529651,-0.012318283097,0.016421318697));
#17869=CARTESIAN_POINT('',(-0.036874593816,-0.011968966814,0.016456352488));
#17870=CARTESIAN_POINT('',(-0.036581516731,-0.012035273907,0.016607435016));
#17871=CARTESIAN_POINT('',(-0.036614786195,-0.012333668079,0.016455801366));
#17872=CARTESIAN_POINT('',(-0.036937968442,-0.012007462527,0.016547866518));
#17873=CARTESIAN_POINT('',(-0.03663781018,-0.012067727143,0.016704386433));
#17874=CARTESIAN_POINT('',(-0.03667816082,-0.012377374469,0.016560205216));
#17875=CARTESIAN_POINT('',(-0.03697969206,-0.01203028214,0.016609980557));
#17876=CARTESIAN_POINT('',(-0.036674489896,-0.012086090141,0.016769529197));
#17877=CARTESIAN_POINT('',(-0.036719884461,-0.012403252403,0.016631080369));
#17878=CARTESIAN_POINT('',(-0.037020900622,-0.012050241607,0.016673198758));
#17879=CARTESIAN_POINT('',(-0.036710197303,-0.012101269023,0.016834819376));
#17880=CARTESIAN_POINT('',(-0.036761093001,-0.012425852784,0.016703226885));
#17881=CARTESIAN_POINT('',(-0.0370209006219633,-0.0123363218309527,0.0165828765281445));
#17882=CARTESIAN_POINT('',(-0.0363829297000878,-0.00764796150808045,0.0180063760900247));
#17883=CARTESIAN_POINT('',(-0.0370209006725265,-0.0120502416314727,0.016673198835513));
#17884=CARTESIAN_POINT('',(-0.0367101973471479,-0.0121012690417669,0.0168348194567234));
#17885=CARTESIAN_POINT('',(-0.0367610930515268,-0.0124258528117109,0.0167032269734606));
#17886=CARTESIAN_POINT('',(-0.037103317012847,-0.0120901601826742,0.0167996340374687));
#17887=CARTESIAN_POINT('',(-0.0367834353017993,-0.0121324018021573,0.0169687333890696));
#17888=CARTESIAN_POINT('',(-0.0368435097848469,-0.0124710533801557,0.0168475194030382));
#17889=CARTESIAN_POINT('',(-0.0371836845969985,-0.012118723833302,0.0169304571286969));
#17890=CARTESIAN_POINT('',(-0.036852619292111,-0.0121502141620385,0.0171032960490522));
#17891=CARTESIAN_POINT('',(-0.0369238769759985,-0.0125032416596733,0.016996863092627));
#17892=CARTESIAN_POINT('',(-0.037301116085,-0.012142960991,0.017133757444));
#17893=CARTESIAN_POINT('',(-0.03695137278,-0.012158036728,0.017307056189));
#17894=CARTESIAN_POINT('',(-0.037041308464,-0.012530204072,0.017229010285));
#17895=CARTESIAN_POINT('',(-0.037339424126,-0.012147832408,0.017202180744));
#17896=CARTESIAN_POINT('',(-0.036983551057,-0.01215730462,0.01737562732));
#17897=CARTESIAN_POINT('',(-0.037079616505,-0.012535518531,0.017307152903));
#17898=CARTESIAN_POINT('',(-0.037413681214,-0.012151009491,0.017339044018));
#17899=CARTESIAN_POINT('',(-0.037045412802,-0.012149475489,0.017511610772));
#17900=CARTESIAN_POINT('',(-0.037153873593,-0.012538634267,0.017463477304));
#17901=CARTESIAN_POINT('',(-0.037449744946,-0.012149340492,0.017407681576));
#17902=CARTESIAN_POINT('',(-0.037075133644,-0.012142279398,0.017579166281));
#17903=CARTESIAN_POINT('',(-0.037189937325,-0.012536463788,0.017541884702));
#17904=CARTESIAN_POINT('',(-0.037519742735,-0.012139323808,0.017545357834));
#17905=CARTESIAN_POINT('',(-0.037132298021,-0.012121588311,0.017713430993));
#17906=CARTESIAN_POINT('',(-0.037259935114,-0.012524478835,0.017699177365));
#17907=CARTESIAN_POINT('',(-0.037553677068,-0.012130977326,0.017614396504));
#17908=CARTESIAN_POINT('',(-0.037159681014,-0.012107993462,0.017780075124));
#17909=CARTESIAN_POINT('',(-0.037293869447,-0.012514665743,0.017778062592));
#17910=CARTESIAN_POINT('',(-0.037602938649,-0.0121131804,0.017718254592));
#17911=CARTESIAN_POINT('',(-0.037198872381,-0.012082909484,0.01787893623));
#17912=CARTESIAN_POINT('',(-0.037343131027,-0.012493905947,0.017896748231));
#17913=CARTESIAN_POINT('',(-0.037619085386,-0.012106366928,0.017752924047));
#17914=CARTESIAN_POINT('',(-0.037211691522,-0.012073695505,0.01791189675));
#17915=CARTESIAN_POINT('',(-0.037359277765,-0.012485977458,0.017936369838));
#17916=CARTESIAN_POINT('',(-0.037650817756,-0.012090910276,0.017822364053));
#17917=CARTESIAN_POINT('',(-0.037236742776,-0.012053626329,0.017977570801));
#17918=CARTESIAN_POINT('',(-0.037391010135,-0.012468026175,0.018015733672));
#17919=CARTESIAN_POINT('',(-0.037666411882,-0.012082254089,0.017857158743));
#17920=CARTESIAN_POINT('',(-0.037248972401,-0.012042747188,0.018010293639));
#17921=CARTESIAN_POINT('',(-0.037406604261,-0.012457988408,0.018055503508));
#17922=CARTESIAN_POINT('',(-0.037742059103,-0.012034811789,0.018029350412));
#17923=CARTESIAN_POINT('',(-0.037308672836,-0.011984184277,0.018173339907));
#17924=CARTESIAN_POINT('',(-0.037482251481,-0.012403043831,0.018252328917));
#17925=CARTESIAN_POINT('',(-0.037795953594,-0.0119833468,0.018163051804));
#17926=CARTESIAN_POINT('',(-0.037349209561,-0.01192624568,0.018295048154));
#17927=CARTESIAN_POINT('',(-0.037536145973,-0.012343640815,0.018405198115));
#17928=CARTESIAN_POINT('',(-0.037866774638,-0.011884976998,0.018357148242));
#17929=CARTESIAN_POINT('',(-0.037401307565,-0.01182386073,0.018467879798));
#17930=CARTESIAN_POINT('',(-0.037606967016,-0.012230324528,0.018627184794));
#17931=CARTESIAN_POINT('',(-0.037888699602,-0.011848634259,0.018420763928));
#17932=CARTESIAN_POINT('',(-0.037417279271,-0.011786751401,0.018524231365));
#17933=CARTESIAN_POINT('',(-0.037628891981,-0.012188489579,0.018699952716));
#17934=CARTESIAN_POINT('',(-0.037918925522,-0.011788411713,0.018514434973));
#17935=CARTESIAN_POINT('',(-0.037439020962,-0.011726989924,0.018606332456));
#17936=CARTESIAN_POINT('',(-0.037659117901,-0.012119208257,0.018807118231));
#17937=CARTESIAN_POINT('',(-0.037928582819,-0.011767311068,0.018545460028));
#17938=CARTESIAN_POINT('',(-0.037445936687,-0.011706228285,0.018633469683));
#17939=CARTESIAN_POINT('',(-0.037668775198,-0.01209494007,0.018842615969));
#17940=CARTESIAN_POINT('',(-0.037946745879,-0.011723686791,0.018606120592));
#17941=CARTESIAN_POINT('',(-0.037458875717,-0.011663774496,0.018686340803));
#17942=CARTESIAN_POINT('',(-0.037686938258,-0.012044779429,0.018912028045));
#17943=CARTESIAN_POINT('',(-0.03795527555,-0.011701127516,0.01863582313));
#17944=CARTESIAN_POINT('',(-0.037464908394,-0.011642051742,0.018712112891));
#17945=CARTESIAN_POINT('',(-0.037695467929,-0.012018845928,0.018946019049));
#17946=CARTESIAN_POINT('',(-0.037995201404,-0.011584625415,0.018781219738));
#17947=CARTESIAN_POINT('',(-0.037493219634,-0.01153014651,0.018838837483));
#17948=CARTESIAN_POINT('',(-0.037735393783,-0.011884946284,0.019112424772));
#17949=CARTESIAN_POINT('',(-0.03801852767,-0.011479690222,0.018887669477));
#17950=CARTESIAN_POINT('',(-0.037508976952,-0.011433957386,0.018929023907));
#17951=CARTESIAN_POINT('',(-0.037758720049,-0.011764426365,0.019234309833));
#17952=CARTESIAN_POINT('',(-0.038040144091,-0.011303793235,0.019031755487));
#17953=CARTESIAN_POINT('',(-0.037523624808,-0.011276525335,0.019052132642));
#17954=CARTESIAN_POINT('',(-0.03778033647,-0.011562515578,0.019399384648));
#17955=CARTESIAN_POINT('',(-0.038045091154,-0.011241659818,0.019077372673));
#17956=CARTESIAN_POINT('',(-0.037526947936,-0.011221473817,0.019091228452));
#17957=CARTESIAN_POINT('',(-0.037785283533,-0.011491209999,0.019451665162));
#17958=CARTESIAN_POINT('',(-0.038050108278,-0.011114326029,0.019160771595));
#17959=CARTESIAN_POINT('',(-0.037530327064,-0.011109308985,0.019163421876));
#17960=CARTESIAN_POINT('',(-0.037790300657,-0.011345109716,0.019547286114));
#17961=CARTESIAN_POINT('',(-0.038050243047,-0.011048838426,0.019198846514));
#17962=CARTESIAN_POINT('',(-0.037530417095,-0.011052089911,0.019196655463));
#17963=CARTESIAN_POINT('',(-0.037790435426,-0.011269985121,0.019590962239));
#17964=CARTESIAN_POINT('',(-0.038045857381,-0.010914292279,0.019267887587));
#17965=CARTESIAN_POINT('',(-0.037527464034,-0.01093462983,0.019257973428));
#17966=CARTESIAN_POINT('',(-0.03778604976,-0.011115665703,0.019670206775));
#17967=CARTESIAN_POINT('',(-0.038041336883,-0.010845233676,0.019298853626));
#17968=CARTESIAN_POINT('',(-0.037524429559,-0.010874566119,0.019285974336));
#17969=CARTESIAN_POINT('',(-0.037781529262,-0.011036470818,0.019705775052));
#17970=CARTESIAN_POINT('',(-0.038027559938,-0.010703495215,0.019353576094));
#17971=CARTESIAN_POINT('',(-0.037515080889,-0.010750844555,0.019336843363));
#17972=CARTESIAN_POINT('',(-0.037767752317,-0.010873951929,0.019768689912));
#17973=CARTESIAN_POINT('',(-0.038018235775,-0.010630560705,0.019377346763));
#17974=CARTESIAN_POINT('',(-0.037508746133,-0.010687144809,0.019359690396));
#17975=CARTESIAN_POINT('',(-0.037758428154,-0.010790336157,0.019796053532));
#17976=CARTESIAN_POINT('',(-0.037983863425,-0.010411968137,0.019436057889));
#17977=CARTESIAN_POINT('',(-0.037485152239,-0.010495505976,0.019418486321));
#17978=CARTESIAN_POINT('',(-0.037724055805,-0.010539762158,0.019863756543));
#17979=CARTESIAN_POINT('',(-0.03795238138,-0.010264782581,0.019459321592));
#17980=CARTESIAN_POINT('',(-0.037463427014,-0.010365206315,0.0194459996));
#17981=CARTESIAN_POINT('',(-0.037692573758,-0.010371083162,0.019890768551));
#17982=CARTESIAN_POINT('',(-0.037902538675,-0.010079089663,0.019469374787));
#17983=CARTESIAN_POINT('',(-0.037427207905,-0.010194849921,0.0194650503));
#17984=CARTESIAN_POINT('',(-0.037642731053,-0.010158316591,0.019902820673));
#17985=CARTESIAN_POINT('',(-0.0378920119,-0.010041777162,0.019470420515));
#17986=CARTESIAN_POINT('',(-0.037419583631,-0.010160752482,0.019468052396));
#17987=CARTESIAN_POINT('',(-0.037632204279,-0.010115566184,0.019904130213));
#17988=CARTESIAN_POINT('',(-0.037870126119,-0.009967782025,0.019470585011));
#17989=CARTESIAN_POINT('',(-0.0374036129810001,-0.010092740755,0.019472397637));
#17990=CARTESIAN_POINT('',(-0.037610318498,-0.01003079121,0.019904547896));
#17991=CARTESIAN_POINT('',(-0.037858748966,-0.009931022823,0.019469712501));
#17992=CARTESIAN_POINT('',(-0.037395262434,-0.010058774628,0.019473761339));
#17993=CARTESIAN_POINT('',(-0.037598941345,-0.009988678904,0.019903666229));
#17994=CARTESIAN_POINT('',(-0.037823348421,-0.009821438911,0.019464328495));
#17995=CARTESIAN_POINT('',(-0.037369172913,-0.009957259452,0.01947541277));
#17996=CARTESIAN_POINT('',(-0.0375635408,-0.009863142675,0.019897861604));
#17997=CARTESIAN_POINT('',(-0.037798059306,-0.009749306074,0.019457057728));
#17998=CARTESIAN_POINT('',(-0.037350277137,-0.009889495687,0.019473344227));
#17999=CARTESIAN_POINT('',(-0.037538251684,-0.009780517328,0.019889787243));
#18000=CARTESIAN_POINT('',(-0.037744193093,-0.009606821654,0.019435479151));
#18001=CARTESIAN_POINT('',(-0.037309379895,-0.00975396796900001,0.019462636177));
#18002=CARTESIAN_POINT('',(-0.037484385472,-0.009617322054,0.019865602347));
#18003=CARTESIAN_POINT('',(-0.037715615604,-0.009536470315,0.019421170251));
#18004=CARTESIAN_POINT('',(-0.037287455068,-0.009686309278,0.019454099651));
#18005=CARTESIAN_POINT('',(-0.037455807983,-0.00953675241,0.019849490561));
#18006=CARTESIAN_POINT('',(-0.037670271841,-0.009432272932,0.019394506946));
#18007=CARTESIAN_POINT('',(-0.037251993154,-0.009584454943,0.019436123721));
#18008=CARTESIAN_POINT('',(-0.03741046422,-0.009417432004,0.019819385249));
#18009=CARTESIAN_POINT('',(-0.037654725402,-0.009397729381,0.019384735691));
#18010=CARTESIAN_POINT('',(-0.037239813053,-0.009550627271,0.01942931378));
#18011=CARTESIAN_POINT('',(-0.037394917781,-0.009377876793,0.019808341439));
#18012=CARTESIAN_POINT('',(-0.037623119912,-0.009329767162,0.019363680484));
#18013=CARTESIAN_POINT('',(-0.037214887215,-0.00948368581700001,0.019414133917));
#18014=CARTESIAN_POINT('',(-0.037363312291,-0.00930005825,0.019784524364));
#18015=CARTESIAN_POINT('',(-0.037607024828,-0.009296262741,0.019352376907));
#18016=CARTESIAN_POINT('',(-0.037202122033,-0.00945049394300001,0.019405766262));
#18017=CARTESIAN_POINT('',(-0.037347217206,-0.009261696717,0.019771728968));
#18018=CARTESIAN_POINT('',(-0.037525118351,-0.009131050827,0.019292111621));
#18019=CARTESIAN_POINT('',(-0.037137549676,-0.009287907011,0.019360578083));
#18020=CARTESIAN_POINT('',(-0.03726531073,-0.009072543594,0.019703469308));
#18021=CARTESIAN_POINT('',(-0.037455051799,-0.009006209944,0.019232012958));
#18022=CARTESIAN_POINT('',(-0.037080651573,-0.009160611098,0.01931215418));
#18023=CARTESIAN_POINT('',(-0.037195244178,-0.008929642002,0.01963527735));
#18024=CARTESIAN_POINT('',(-0.037343235527,-0.00882937501,0.019125190743));
#18025=CARTESIAN_POINT('',(-0.036986748025,-0.008975129884,0.019219634813));
#18026=CARTESIAN_POINT('',(-0.037083427906,-0.008727272424,0.019513936502));
#18027=CARTESIAN_POINT('',(-0.03730475018,-0.008772089632,0.019086679248));
#18028=CARTESIAN_POINT('',(-0.03695443279,-0.008914916629,0.019185945236));
#18029=CARTESIAN_POINT('',(-0.037044942559,-0.008661723823,0.019470171615));
#18030=CARTESIAN_POINT('',(-0.03722687049,-0.008662929292,0.019005550035));
#18031=CARTESIAN_POINT('',(-0.036888415857,-0.00879911653500001,0.019113533106));
#18032=CARTESIAN_POINT('',(-0.036967062869,-0.008536835522,0.01937794176));
#18033=CARTESIAN_POINT('',(-0.037187320072,-0.008610791877,0.018962790615));
#18034=CARTESIAN_POINT('',(-0.036854627768,-0.008743216033,0.019074796792));
#18035=CARTESIAN_POINT('',(-0.036927512451,-0.008477195434,0.019329315909));
#18036=CARTESIAN_POINT('',(-0.03706685504,-0.008461415123,0.018828228599));
#18037=CARTESIAN_POINT('',(-0.036751742399,-0.00858303382199999,0.018951988873));
#18038=CARTESIAN_POINT('',(-0.036807047419,-0.008306352736,0.019176249766));
#18039=CARTESIAN_POINT('',(-0.03698413842,-0.00837115601,0.018730193296));
#18040=CARTESIAN_POINT('',(-0.036679594089,-0.00848315825100001,0.018859845872));
#18041=CARTESIAN_POINT('',(-0.036724330798,-0.008203164137,0.019064679358));
#18042=CARTESIAN_POINT('',(-0.036813690053,-0.008209181877,0.018517719676));
#18043=CARTESIAN_POINT('',(-0.036528822624,-0.00830111902100001,0.018655023827));
#18044=CARTESIAN_POINT('',(-0.036553882432,-0.008018087581,0.018822772918));
#18045=CARTESIAN_POINT('',(-0.03672806298,-0.008139470644,0.018405905936));
#18046=CARTESIAN_POINT('',(-0.0364522190969999,-0.00822060741400001,0.018545456308));
#18047=CARTESIAN_POINT('',(-0.036468255359,-0.007938489295,0.018695425021));
#18048=CARTESIAN_POINT('',(-0.036556082968,-0.008021465132,0.01817201132));
#18049=CARTESIAN_POINT('',(-0.036296957641,-0.008081939279,0.018312490038));
#18050=CARTESIAN_POINT('',(-0.036296275347,-0.00780388162,0.018428951735));
#18051=CARTESIAN_POINT('',(-0.036469700557,-0.007973146042,0.018049892539));
#18052=CARTESIAN_POINT('',(-0.036218299035,-0.008023023348,0.018189430236));
#18053=CARTESIAN_POINT('',(-0.03620989256,-0.007748843646,0.018289782591));
#18054=CARTESIAN_POINT('',(-0.0363829297,-0.007935966222,0.017922392252));
#18055=CARTESIAN_POINT('',(-0.036137554584,-0.00797535009500001,0.01805745087));
#18056=CARTESIAN_POINT('',(-0.036123122079,-0.007706601765,0.018144438831));
#18057=CARTESIAN_POINT('',(-0.0387712812904549,-1.29145307733547E-11,1.90092953692937E-11));
#18058=CARTESIAN_POINT('',(-0.0363829297,-0.019489230098,0.002088447775));
#18059=CARTESIAN_POINT('',(-0.036137554584,-0.019625886228,0.002121869649));
#18060=CARTESIAN_POINT('',(-0.036123122079,-0.019566845848,0.00239810651));
#18061=CARTESIAN_POINT('',(-0.036296388628,-0.019360563338,0.002056979854));
#18062=CARTESIAN_POINT('',(-0.036059352191,-0.019492100962,0.002097943941));
#18063=CARTESIAN_POINT('',(-0.03603658062,-0.019420241494,0.00236211242));
#18064=CARTESIAN_POINT('',(-0.036211750879,-0.019236205228,0.002014072051));
#18065=CARTESIAN_POINT('',(-0.03598108599,-0.019359587151,0.002061252005));
#18066=CARTESIAN_POINT('',(-0.035951943258,-0.019278561257,0.002312976363));
#18067=CARTESIAN_POINT('',(-0.036046427611,-0.01899593144,0.001905705907));
#18068=CARTESIAN_POINT('',(-0.03582764111,-0.019102466172,0.00196200056));
#18069=CARTESIAN_POINT('',(-0.03578661999,-0.019004843948,0.002188783069));
#18070=CARTESIAN_POINT('',(-0.035965731891,-0.018880003958,0.001840264492));
#18071=CARTESIAN_POINT('',(-0.035752240428,-0.018977419333,0.001900058743));
#18072=CARTESIAN_POINT('',(-0.03570592427,-0.018872794113,0.002113745518));
#18073=CARTESIAN_POINT('',(-0.035867783855,-0.018740766939,0.001742981965));
#18074=CARTESIAN_POINT('',(-0.035659677357,-0.018825445883,0.00180418218));
#18075=CARTESIAN_POINT('',(-0.035607976234,-0.018714208906,0.002002145766));
#18076=CARTESIAN_POINT('',(-0.03584830488,-0.018713153198,0.001722699015));
#18077=CARTESIAN_POINT('',(-0.035641412325,-0.018795533693,0.001784265567));
#18078=CARTESIAN_POINT('',(-0.035588497259,-0.018682758826,0.001978875521));
#18079=CARTESIAN_POINT('',(-0.035810061793,-0.018659082064,0.0016809538));
#18080=CARTESIAN_POINT('',(-0.035605524332,-0.018736905391,0.0017430598));
#18081=CARTESIAN_POINT('',(-0.035550254172,-0.018621177248,0.001930977518));
#18082=CARTESIAN_POINT('',(-0.035791254693,-0.018632563266,0.001659452537));
#18083=CARTESIAN_POINT('',(-0.035587855191,-0.018708112389,0.001721737929));
#18084=CARTESIAN_POINT('',(-0.035531447072,-0.018590975808,0.001906305033));
#18085=CARTESIAN_POINT('',(-0.035735788251,-0.018554552292,0.001593061423));
#18086=CARTESIAN_POINT('',(-0.035535852231,-0.018623571688,0.001655788575));
#18087=CARTESIAN_POINT('',(-0.03547598063,-0.018502133765,0.001830115341));
#18088=CARTESIAN_POINT('',(-0.035700081089,-0.018504601769,0.00154628902));
#18089=CARTESIAN_POINT('',(-0.035502196601,-0.018569127867,0.001608840169));
#18090=CARTESIAN_POINT('',(-0.035440273468,-0.018445251153,0.001776431383));
#18091=CARTESIAN_POINT('',(-0.035596955729,-0.01836101404,0.001398258712));
#18092=CARTESIAN_POINT('',(-0.035405412743,-0.018413252525,0.001459938607));
#18093=CARTESIAN_POINT('',(-0.035337148108,-0.018281744346,0.001606500757));
#18094=CARTESIAN_POINT('',(-0.035533471872,-0.018273557744,0.001289394297));
#18095=CARTESIAN_POINT('',(-0.03534514464,-0.018317127379,0.001348630596));
#18096=CARTESIAN_POINT('',(-0.035273664252,-0.018182166802,0.001481497731));
#18097=CARTESIAN_POINT('',(-0.035462076716,-0.01817592941,0.001138664356));
#18098=CARTESIAN_POINT('',(-0.035277056499,-0.018209299086,0.001192172175));
#18099=CARTESIAN_POINT('',(-0.035202269094,-0.018071016536,0.001308380108));
#18100=CARTESIAN_POINT('',(-0.035448157312,-0.018156936087,0.00110767252));
#18101=CARTESIAN_POINT('',(-0.035263851039,-0.018188427631,0.001160131862));
#18102=CARTESIAN_POINT('',(-0.035188349691,-0.018049393067,0.001272783163));
#18103=CARTESIAN_POINT('',(-0.035421421576,-0.018120522953,0.001044695664));
#18104=CARTESIAN_POINT('',(-0.035238481118,-0.01814840061,0.001094908468));
#18105=CARTESIAN_POINT('',(-0.035161613954,-0.018007938413,0.001200444691));
#18106=CARTESIAN_POINT('',(-0.035408615027,-0.01810311612,0.001012747602));
#18107=CARTESIAN_POINT('',(-0.035226318844,-0.018129247863,0.001061759551));
#18108=CARTESIAN_POINT('',(-0.035148807406,-0.017988121995,0.001163745631));
#18109=CARTESIAN_POINT('',(-0.035371903227,-0.018053301561,0.000915516155));
#18110=CARTESIAN_POINT('',(-0.035191509303,-0.018074518308,0.000960895819));
#18111=CARTESIAN_POINT('',(-0.035112095605,-0.01793141283,0.001052049584));
#18112=CARTESIAN_POINT('',(-0.035349701075,-0.018023292834,0.000848849473));
#18113=CARTESIAN_POINT('',(-0.035170375015,-0.018041410365,0.000891381795));
#18114=CARTESIAN_POINT('',(-0.035089893455,-0.017897252254,0.000975458269));
#18115=CARTESIAN_POINT('',(-0.035310076825,-0.017969873141,0.000711689247));
#18116=CARTESIAN_POINT('',(-0.035132682741,-0.01798250627,0.00074809069));
#18117=CARTESIAN_POINT('',(-0.035050269204,-0.01783644352,0.000817866864));
#18118=CARTESIAN_POINT('',(-0.035292653375,-0.01794646038,0.000641196756));
#18119=CARTESIAN_POINT('',(-0.035116074086,-0.017956629983,0.000674242814));
#18120=CARTESIAN_POINT('',(-0.035032845755,-0.017809793311,0.000736867981));
#18121=CARTESIAN_POINT('',(-0.035270404132,-0.017916617409,0.000532382892));
#18122=CARTESIAN_POINT('',(-0.035094864144,-0.017923641781,0.000560006423));
#18123=CARTESIAN_POINT('',(-0.03501059651,-0.017775824484,0.00061182896));
#18124=CARTESIAN_POINT('',(-0.03526362249,-0.017907532057,0.000495486354));
#18125=CARTESIAN_POINT('',(-0.035088401673,-0.017913601835,0.000521272544));
#18126=CARTESIAN_POINT('',(-0.035003814869,-0.017765483208,0.000569429626));
#18127=CARTESIAN_POINT('',(-0.035251577427,-0.017891408044,0.000421626354));
#18128=CARTESIAN_POINT('',(-0.035076925826,-0.017895786451,0.000443697364));
#18129=CARTESIAN_POINT('',(-0.034991769806,-0.017747130448,0.000484552102));
#18130=CARTESIAN_POINT('',(-0.035246291308,-0.01788433888,0.000384573767));
#18131=CARTESIAN_POINT('',(-0.035071886429,-0.017887970471,0.000404748673));
#18132=CARTESIAN_POINT('',(-0.034986483687,-0.017739084243,0.000441971503));
#18133=CARTESIAN_POINT('',(-0.035223521483,-0.017853905806,0.00019870341));
#18134=CARTESIAN_POINT('',(-0.035050225188,-0.017854392227,0.000209670015));
#18135=CARTESIAN_POINT('',(-0.034963713862,-0.017704445198,0.000228366787));
#18136=CARTESIAN_POINT('',(-0.035216913712,-0.017845112687,4.808316E-5));
#18137=CARTESIAN_POINT('',(-0.035043883179,-0.017844601077,5.0495546E-5));
#18138=CARTESIAN_POINT('',(-0.034957106091,-0.017694437363,5.5260102E-5));
#18139=CARTESIAN_POINT('',(-0.035223876434,-0.017854401084,-0.000142705112));
#18140=CARTESIAN_POINT('',(-0.035050518048,-0.017854867848,-0.00015026669));
#18141=CARTESIAN_POINT('',(-0.034964068813,-0.017705009213,-0.000164006944));
#18142=CARTESIAN_POINT('',(-0.03522604562,-0.017857295098,-0.000181008826));
#18143=CARTESIAN_POINT('',(-0.035052587043,-0.017858069693,-0.000190597666));
#18144=CARTESIAN_POINT('',(-0.034966237999,-0.01770830312,-0.000208027982));
#18145=CARTESIAN_POINT('',(-0.035231850552,-0.017865043926,-0.000256731481));
#18146=CARTESIAN_POINT('',(-0.035058120997,-0.017866638035,-0.000270288381));
#18147=CARTESIAN_POINT('',(-0.034972042931,-0.017717122731,-0.00029505227));
#18148=CARTESIAN_POINT('',(-0.0352354894,-0.01786990288,-0.000294294755));
#18149=CARTESIAN_POINT('',(-0.035061591095,-0.017872012494,-0.000309815542));
#18150=CARTESIAN_POINT('',(-0.034975681779,-0.01772265315,-0.0003382214));
#18151=CARTESIAN_POINT('',(-0.035248550352,-0.017887356278,-0.000406114618));
#18152=CARTESIAN_POINT('',(-0.035074046816,-0.017891317393,-0.000427475545));
#18153=CARTESIAN_POINT('',(-0.034988742731,-0.01774251863,-0.000466726903));
#18154=CARTESIAN_POINT('',(-0.035260111701,-0.017902819307,-0.000479503556));
#18155=CARTESIAN_POINT('',(-0.035085080525,-0.017908432544,-0.000504635436));
#18156=CARTESIAN_POINT('',(-0.03500030408,-0.017760118859,-0.000551064032));
#18157=CARTESIAN_POINT('',(-0.035281577861,-0.017931602322,-0.000587901928));
#18158=CARTESIAN_POINT('',(-0.035105505104,-0.017940189326,-0.000618239168));
#18159=CARTESIAN_POINT('',(-0.03502177024,-0.017792881061,-0.000675626671));
#18160=CARTESIAN_POINT('',(-0.035289421938,-0.017942130116,-0.000623753285));
#18161=CARTESIAN_POINT('',(-0.035112977015,-0.017951817298,-0.000655825409));
#18162=CARTESIAN_POINT('',(-0.035029614317,-0.017804864435,-0.000716823028));
#18163=CARTESIAN_POINT('',(-0.035306476701,-0.017965050902,-0.000694894802));
#18164=CARTESIAN_POINT('',(-0.035129211644,-0.017977114049,-0.000730326682));
#18165=CARTESIAN_POINT('',(-0.03504666908,-0.017830954681,-0.000798568263));
#18166=CARTESIAN_POINT('',(-0.035315718145,-0.017977485365,-0.000730290044));
#18167=CARTESIAN_POINT('',(-0.035138009535,-0.017990837846,-0.000767363366));
#18168=CARTESIAN_POINT('',(-0.035055910524,-0.017845108762,-0.000839237874));
#18169=CARTESIAN_POINT('',(-0.035345244257,-0.018017274364,-0.000834778442));
#18170=CARTESIAN_POINT('',(-0.035166136457,-0.018034776161,-0.000876705266000001));
#18171=CARTESIAN_POINT('',(-0.035085436637,-0.017890401172,-0.000959292019));
#18172=CARTESIAN_POINT('',(-0.035367258146,-0.018047016063,-0.000902026906));
#18173=CARTESIAN_POINT('',(-0.035187092355,-0.018067591645,-0.000946845463));
#18174=CARTESIAN_POINT('',(-0.035107450524,-0.017924257611,-0.001036552565));
#18175=CARTESIAN_POINT('',(-0.035415540032,-0.01811249853,-0.001032054747));
#18176=CARTESIAN_POINT('',(-0.035232955499,-0.018139667727,-0.001082015991));
#18177=CARTESIAN_POINT('',(-0.035155732411,-0.017998802798,-0.001185925847));
#18178=CARTESIAN_POINT('',(-0.035441809443,-0.018148241136,-0.001094832722));
#18179=CARTESIAN_POINT('',(-0.035257918294,-0.018179017227,-0.001147092497));
#18180=CARTESIAN_POINT('',(-0.035182001822,-0.018039493646,-0.001258036973));
#18181=CARTESIAN_POINT('',(-0.035498359317,-0.018225522805,-0.001216100433));
#18182=CARTESIAN_POINT('',(-0.035311533473,-0.018263877422,-0.001272286645));
#18183=CARTESIAN_POINT('',(-0.035238551696,-0.018127478563,-0.001397318651));
#18184=CARTESIAN_POINT('',(-0.035528803299,-0.018267288112,-0.001274848098));
#18185=CARTESIAN_POINT('',(-0.035340397738,-0.018309728944,-0.001332693764));
#18186=CARTESIAN_POINT('',(-0.035268995678,-0.01817503025,-0.001464785336));
#18187=CARTESIAN_POINT('',(-0.035624302868,-0.018398937175,-0.001441946764));
#18188=CARTESIAN_POINT('',(-0.035431143853,-0.018454527567,-0.001504443888));
#18189=CARTESIAN_POINT('',(-0.035364495247,-0.018324926454,-0.001656660391));
#18190=CARTESIAN_POINT('',(-0.035693625065,-0.018495301896,-0.001541838752));
#18191=CARTESIAN_POINT('',(-0.035496770299,-0.018560086634,-0.001605426885));
#18192=CARTESIAN_POINT('',(-0.035433817443,-0.018434657594,-0.001771331198));
#18193=CARTESIAN_POINT('',(-0.035804878296,-0.018651701588,-0.001676100287));
#18194=CARTESIAN_POINT('',(-0.035600812464,-0.018729153932,-0.001738536628));
#18195=CARTESIAN_POINT('',(-0.035545070675,-0.018612771043,-0.001925410518));
#18196=CARTESIAN_POINT('',(-0.035843360668,-0.01870607504,-0.001718396961));
#18197=CARTESIAN_POINT('',(-0.035636958249,-0.018788171317,-0.001780300456));
#18198=CARTESIAN_POINT('',(-0.035583553047,-0.018674696557,-0.001973941769));
#18199=CARTESIAN_POINT('',(-0.035921655233,-0.018817323726,-0.001796776766));
#18200=CARTESIAN_POINT('',(-0.035710302083,-0.018908539739,-0.001856931323));
#18201=CARTESIAN_POINT('',(-0.035661847612,-0.018801403665,-0.002063858322));
#18202=CARTESIAN_POINT('',(-0.035961464931,-0.018874192105,-0.001832902387));
#18203=CARTESIAN_POINT('',(-0.035747535996,-0.018969953338,-0.00189179072));
#18204=CARTESIAN_POINT('',(-0.035701657309,-0.018866177417,-0.002105292476));
#18205=CARTESIAN_POINT('',(-0.036082708725,-0.019048372444,-0.001932563921));
#18206=CARTESIAN_POINT('',(-0.035861344783,-0.019158636987,-0.001987306041));
#18207=CARTESIAN_POINT('',(-0.035822901104,-0.019064581187,-0.00221957399));
#18208=CARTESIAN_POINT('',(-0.036165937985,-0.019169231525,-0.001987458368));
#18209=CARTESIAN_POINT('',(-0.035938765603,-0.019288313365,-0.002037355517));
#18210=CARTESIAN_POINT('',(-0.035906130364,-0.019202261747,-0.00228248524));
#18211=CARTESIAN_POINT('',(-0.036272749616,-0.019326186492,-0.002041954834));
#18212=CARTESIAN_POINT('',(-0.036036325391,-0.019453445768,-0.002083965382));
#18213=CARTESIAN_POINT('',(-0.036012941995,-0.019381080036,-0.002344895831));
#18214=CARTESIAN_POINT('',(-0.036294271622,-0.019357902787,-0.002052147118));
#18215=CARTESIAN_POINT('',(-0.036056160144,-0.019487107185,-0.002092585706));
#18216=CARTESIAN_POINT('',(-0.036034464001,-0.019417215175,-0.002356565423));
#18217=CARTESIAN_POINT('',(-0.036337241164,-0.019421408713,-0.002070948756));
#18218=CARTESIAN_POINT('',(-0.036095695252,-0.019554376812,-0.002108113551));
#18219=CARTESIAN_POINT('',(-0.036077433543,-0.019489570721,-0.002378086456));
#18220=CARTESIAN_POINT('',(-0.036358730845,-0.019453260076,-0.002079581263));
#18221=CARTESIAN_POINT('',(-0.03611543566,-0.019588053885,-0.00211503004));
#18222=CARTESIAN_POINT('',(-0.036098923223,-0.019525861458,-0.002387964418));
#18223=CARTESIAN_POINT('',(-0.036423211553,-0.019549105164,-0.002103217759));
#18224=CARTESIAN_POINT('',(-0.036174782484,-0.019689559821,-0.002133392794));
#18225=CARTESIAN_POINT('',(-0.036163403931,-0.019635067732,-0.002415001427));
#18226=CARTESIAN_POINT('',(-0.036466213928,-0.019613389425,-0.002115965485));
#18227=CARTESIAN_POINT('',(-0.036214084658,-0.01975713597,-0.002142252449));
#18228=CARTESIAN_POINT('',(-0.036206406307,-0.019708316806,-0.002429569065));
#18229=CARTESIAN_POINT('',(-0.036595254777,-0.019807388917,-0.002145346512));
#18230=CARTESIAN_POINT('',(-0.03633245937,-0.019961690258,-0.002159474874));
#18231=CARTESIAN_POINT('',(-0.036335447156,-0.019929380277,-0.002463096114));
#18232=CARTESIAN_POINT('',(-0.036681322249,-0.019938243356,-0.002153193167));
#18233=CARTESIAN_POINT('',(-0.036410235723,-0.020097509831,-0.00215769725));
#18234=CARTESIAN_POINT('',(-0.036421514628,-0.020078502366,-0.002471966356));
#18235=CARTESIAN_POINT('',(-0.03678899075,-0.020103771553,-0.002147749667));
#18236=CARTESIAN_POINT('',(-0.036505370032,-0.020265213313,-0.002139955671));
#18237=CARTESIAN_POINT('',(-0.036529183129,-0.02026715354,-0.002465549917));
#18238=CARTESIAN_POINT('',(-0.036810556304,-0.020137018306,-0.002145885901));
#18239=CARTESIAN_POINT('',(-0.036524605066,-0.020299204976,-0.002135530565));
#18240=CARTESIAN_POINT('',(-0.036550748683,-0.020305045337,-0.002463377054));
#18241=CARTESIAN_POINT('',(-0.036853337272,-0.020203152393,-0.00214063762));
#18242=CARTESIAN_POINT('',(-0.036562661331,-0.020366616451,-0.002125129214));
#18243=CARTESIAN_POINT('',(-0.036593529651,-0.020380420704,-0.002457286744));
#18244=CARTESIAN_POINT('',(-0.036874593816,-0.020236102715,-0.002137253074));
#18245=CARTESIAN_POINT('',(-0.036581516731,-0.020400097569,-0.002119135437));
#18246=CARTESIAN_POINT('',(-0.036614786195,-0.020417976062,-0.002453369195));
#18247=CARTESIAN_POINT('',(-0.036937968442,-0.020334604047,-0.002124834324));
#18248=CARTESIAN_POINT('',(-0.03663781018,-0.020500286578,-0.002098765055));
#18249=CARTESIAN_POINT('',(-0.03667816082,-0.020530245644,-0.002439018114));
#18250=CARTESIAN_POINT('',(-0.03697969206,-0.020399806189,-0.002113539669));
#18251=CARTESIAN_POINT('',(-0.036674489896,-0.020565883365,-0.002082096496));
#18252=CARTESIAN_POINT('',(-0.036719884461,-0.020604564293,-0.002425991486));
#18253=CARTESIAN_POINT('',(-0.037020900622,-0.020464534491,-0.002099215974));
#18254=CARTESIAN_POINT('',(-0.036710197303,-0.02063001576,-0.002062596704));
#18255=CARTESIAN_POINT('',(-0.036761093001,-0.0206783452,-0.002409490732));
#18256=CARTESIAN_POINT('',(-0.0370209006221877,-0.0205293532570174,-0.00239212983048223));
#18257=CARTESIAN_POINT('',(-0.0363829297001963,-0.019417959879229,0.00237985909232116));
#18258=CARTESIAN_POINT('',(-0.0370209006725265,-0.0204645345703645,-0.00209921595643747));
#18259=CARTESIAN_POINT('',(-0.0367101973471479,-0.0206300158392919,-0.00206259667989087));
#18260=CARTESIAN_POINT('',(-0.0367610930515268,-0.0206783452904645,-0.00240949071176802));
#18261=CARTESIAN_POINT('',(-0.037103317012847,-0.0205939899421424,-0.00207056883537586));
#18262=CARTESIAN_POINT('',(-0.0367834353017993,-0.0207615550854043,-0.00202260147516363));
#18263=CARTESIAN_POINT('',(-0.0368435097848469,-0.0208259064844385,-0.00237648933787403));
#18264=CARTESIAN_POINT('',(-0.0371836845969985,-0.0207215678876372,-0.00202989413701114));
#18265=CARTESIAN_POINT('',(-0.036852619292111,-0.0208869959479472,-0.00197074610137332));
#18266=CARTESIAN_POINT('',(-0.0369238769759985,-0.0209713360532264,-0.00232969336136768));
#18267=CARTESIAN_POINT('',(-0.037301116085,-0.020909749705,-0.001949233973));
#18268=CARTESIAN_POINT('',(-0.03695137278,-0.021067368688,-0.001875640572));
#18269=CARTESIAN_POINT('',(-0.037041308464,-0.021185862625,-0.002236969898));
#18270=CARTESIAN_POINT('',(-0.037339424126,-0.020971441729,-0.001919241095));
#18271=CARTESIAN_POINT('',(-0.036983551057,-0.021126386976,-0.001840720983));
#18272=CARTESIAN_POINT('',(-0.037079616505,-0.021256193347,-0.002202501046));
#18273=CARTESIAN_POINT('',(-0.037413681214,-0.021091557342,-0.001853560892));
#18274=CARTESIAN_POINT('',(-0.037045412802,-0.021240237534,-0.00176594903));
#18275=CARTESIAN_POINT('',(-0.037153873593,-0.021393132117,-0.002127037152));
#18276=CARTESIAN_POINT('',(-0.037449744946,-0.021150164712,-0.001817796718));
#18277=CARTESIAN_POINT('',(-0.037075133644,-0.021295144276,-0.001725939277));
#18278=CARTESIAN_POINT('',(-0.037189937325,-0.021459949676,-0.002085953763));
#18279=CARTESIAN_POINT('',(-0.037519742735,-0.021264387507,-0.001740283886));
#18280=CARTESIAN_POINT('',(-0.037132298021,-0.021401075383,-0.001640887915));
#18281=CARTESIAN_POINT('',(-0.037259935114,-0.021590176641,-0.001996928158));
#18282=CARTESIAN_POINT('',(-0.037553677068,-0.021320003507,-0.001698536285));
#18283=CARTESIAN_POINT('',(-0.037159681014,-0.02145199347,-0.001595792365));
#18284=CARTESIAN_POINT('',(-0.037293869447,-0.021653586706,-0.001948987157));
#18285=CARTESIAN_POINT('',(-0.037602938649,-0.021401048787,-0.001631194651));
#18286=CARTESIAN_POINT('',(-0.037198872381,-0.02152506771,-0.00152463845));
#18287=CARTESIAN_POINT('',(-0.037343131027,-0.021745991586,-0.001871665827));
#18288=CARTESIAN_POINT('',(-0.037619085386,-0.02142766668,-0.001607959283));
#18289=CARTESIAN_POINT('',(-0.037211691522,-0.021549005368,-0.00150017865));
#18290=CARTESIAN_POINT('',(-0.037359277765,-0.02177634066,-0.00184498875));
#18291=CARTESIAN_POINT('',(-0.037650817756,-0.021480075164,-0.001559853428));
#18292=CARTESIAN_POINT('',(-0.037236742776,-0.021595846177,-0.001449961208));
#18293=CARTESIAN_POINT('',(-0.037391010135,-0.021836096115,-0.001789760567));
#18294=CARTESIAN_POINT('',(-0.037666411882,-0.021505880156,-0.001534959604));
#18295=CARTESIAN_POINT('',(-0.037248972401,-0.021618745415,-0.001424178176));
#18296=CARTESIAN_POINT('',(-0.037406604261,-0.02186551892,-0.001761182687));
#18297=CARTESIAN_POINT('',(-0.037742059103,-0.021631281365,-0.001407777533));
#18298=CARTESIAN_POINT('',(-0.037308672836,-0.021730666169,-0.001291938074));
#18299=CARTESIAN_POINT('',(-0.037482251481,-0.022008502436,-0.001615186583));
#18300=CARTESIAN_POINT('',(-0.037795953594,-0.021721337673,-0.001296356849));
#18301=CARTESIAN_POINT('',(-0.037349209561,-0.021807099305,-0.001180907653));
#18302=CARTESIAN_POINT('',(-0.037536145973,-0.022111189537,-0.001487307464));
#18303=CARTESIAN_POINT('',(-0.037866774638,-0.021840245218,-0.001114117882));
#18304=CARTESIAN_POINT('',(-0.037401307565,-0.021905583424,-0.001005823865));
#18305=CARTESIAN_POINT('',(-0.037606967016,-0.022246777496,-0.001278179341));
#18306=CARTESIAN_POINT('',(-0.037888699602,-0.021877166648,-0.001050836305));
#18307=CARTESIAN_POINT('',(-0.037417279271,-0.021935830648,-0.000945510459000001));
#18308=CARTESIAN_POINT('',(-0.037628891981,-0.022288878891,-0.001205565251));
#18309=CARTESIAN_POINT('',(-0.037918925522,-0.02192817688,-0.000951846528));
#18310=CARTESIAN_POINT('',(-0.037439020962,-0.02197705154,-0.000852704956));
#18311=CARTESIAN_POINT('',(-0.037659117901,-0.022347046289,-0.001091983109));
#18312=CARTESIAN_POINT('',(-0.037928582819,-0.021944495043,-0.000918060305));
#18313=CARTESIAN_POINT('',(-0.037445936687,-0.021990172249,-0.000821156235));
#18314=CARTESIAN_POINT('',(-0.037668775198,-0.022365654138,-0.001053217373));
#18315=CARTESIAN_POINT('',(-0.037946745879,-0.021975216494,-0.000849950291));
#18316=CARTESIAN_POINT('',(-0.037458875717,-0.022014733087,-0.000757954616));
#18317=CARTESIAN_POINT('',(-0.037686938258,-0.022400686439,-0.000975070946));
#18318=CARTESIAN_POINT('',(-0.03795527555,-0.021989660009,-0.000815562116));
#18319=CARTESIAN_POINT('',(-0.037464908394,-0.022026190993,-0.000726256116));
#18320=CARTESIAN_POINT('',(-0.037695467929,-0.022417156761,-0.000935616373));
#18321=CARTESIAN_POINT('',(-0.037995201404,-0.022057326114,-0.000641970034));
#18322=CARTESIAN_POINT('',(-0.037493219634,-0.022079985093,-0.000565981045));
#18323=CARTESIAN_POINT('',(-0.037735393783,-0.022494318522,-0.000736453018));
#18324=CARTESIAN_POINT('',(-0.03801852767,-0.022097046697,-0.000497868621));
#18325=CARTESIAN_POINT('',(-0.037508976952,-0.022109994265,-0.000437585608));
#18326=CARTESIAN_POINT('',(-0.037758720049,-0.022539614123,-0.000571137177));
#18327=CARTESIAN_POINT('',(-0.038040144091,-0.022133880348,-0.000273494358));
#18328=CARTESIAN_POINT('',(-0.037523624808,-0.022137893532,-0.000239691086));
#18329=CARTESIAN_POINT('',(-0.03778033647,-0.022581617712,-0.000313739898));
#18330=CARTESIAN_POINT('',(-0.038045091154,-0.022142319282,-0.000196876647));
#18331=CARTESIAN_POINT('',(-0.037526947936,-0.022144225738,-0.000172467167));
#18332=CARTESIAN_POINT('',(-0.037785283533,-0.022591241175,-0.000225847199));
#18333=CARTESIAN_POINT('',(-0.038050108278,-0.022150877972,-4.490289E-5));
#18334=CARTESIAN_POINT('',(-0.037530327064,-0.02215066466,-3.9232862E-5));
#18335=CARTESIAN_POINT('',(-0.037790300657,-0.022601001208,-5.1510166E-5));
#18336=CARTESIAN_POINT('',(-0.038050243047,-0.022151108018,3.0848498E-5));
#18337=CARTESIAN_POINT('',(-0.037530417095,-0.022150836255,2.6937103E-5));
#18338=CARTESIAN_POINT('',(-0.037790435426,-0.022601263544,3.5387705E-5));
#18339=CARTESIAN_POINT('',(-0.038045857381,-0.022143626267,0.000181889416));
#18340=CARTESIAN_POINT('',(-0.037527464034,-0.022145209129,0.0001593195));
#18341=CARTESIAN_POINT('',(-0.03778604976,-0.022592731617,0.000208654509));
#18342=CARTESIAN_POINT('',(-0.038041336883,-0.022135914342,0.000257178939));
#18343=CARTESIAN_POINT('',(-0.037524429559,-0.022139426771,0.000225336654));
#18344=CARTESIAN_POINT('',(-0.037781529262,-0.022583937206,0.00029502343));
#18345=CARTESIAN_POINT('',(-0.038027559938,-0.022112436159,0.000407289281));
#18346=CARTESIAN_POINT('',(-0.037515080889,-0.022121619859,0.000357917185));
#18347=CARTESIAN_POINT('',(-0.037767752317,-0.022557163628,0.000467226346));
#18348=CARTESIAN_POINT('',(-0.038018235775,-0.022096554907,0.000482337755));
#18349=CARTESIAN_POINT('',(-0.037508746133,-0.022109556097,0.0004245063));
#18350=CARTESIAN_POINT('',(-0.037758428154,-0.022539053331,0.000553321539));
#18351=CARTESIAN_POINT('',(-0.037983863425,-0.02203810395,0.000701000035));
#18352=CARTESIAN_POINT('',(-0.037485152239,-0.022064655445,0.00061986836));
#18353=CARTESIAN_POINT('',(-0.037724055805,-0.02247239886,0.000804176493));
#18354=CARTESIAN_POINT('',(-0.03795238138,-0.02198465813,0.000840098316));
#18355=CARTESIAN_POINT('',(-0.037463427014,-0.022023332813,0.000746467815999999));
#18356=CARTESIAN_POINT('',(-0.037692573758,-0.022411452447,0.000963762793));
#18357=CARTESIAN_POINT('',(-0.037902538675,-0.021900517993,0.001005939698));
#18358=CARTESIAN_POINT('',(-0.037427207905,-0.021954653006,0.000903526131000001));
#18359=CARTESIAN_POINT('',(-0.037642731053,-0.022315506605,0.001154050109));
#18360=CARTESIAN_POINT('',(-0.0378920119,-0.021882767369,0.001038776136));
#18361=CARTESIAN_POINT('',(-0.037419583631,-0.021940204178,0.000934556427));
#18362=CARTESIAN_POINT('',(-0.037632204279,-0.022295265496,0.001191727817));
#18363=CARTESIAN_POINT('',(-0.037870126119,-0.021845912259,0.001102940053));
#18364=CARTESIAN_POINT('',(-0.037403612981,-0.021909961403,0.000995628931000001));
#18365=CARTESIAN_POINT('',(-0.037610318498,-0.022253239734,0.00126535394));
#18366=CARTESIAN_POINT('',(-0.037858748966,-0.021826777042,0.001134338201));
#18367=CARTESIAN_POINT('',(-0.037395262434,-0.02189415934,0.001025726311));
#18368=CARTESIAN_POINT('',(-0.037598941345,-0.022231420035,0.001301383433));
#18369=CARTESIAN_POINT('',(-0.037823348421,-0.0217673224,0.001226548649));
#18370=CARTESIAN_POINT('',(-0.037369172913,-0.021844831934,0.001114466748));
#18371=CARTESIAN_POINT('',(-0.0375635408,-0.022163624967,0.001407198685));
#18372=CARTESIAN_POINT('',(-0.037798059306,-0.021724959312,0.001285382135));
#18373=CARTESIAN_POINT('',(-0.037350277137,-0.02180915864,0.001172117618));
#18374=CARTESIAN_POINT('',(-0.037538251684,-0.022115319692,0.001474717154));
#18375=CARTESIAN_POINT('',(-0.037744193093,-0.021635029507,0.001397987973));
#18376=CARTESIAN_POINT('',(-0.037309379895,-0.021732121338,0.001284134039));
#18377=CARTESIAN_POINT('',(-0.037484385472,-0.022012777321,0.001603955958));
#18378=CARTESIAN_POINT('',(-0.037715615604,-0.021587461967,0.00145175957));
#18379=CARTESIAN_POINT('',(-0.037287455068,-0.021690899144,0.001338459922));
#18380=CARTESIAN_POINT('',(-0.037455807983,-0.021958539283,0.001665675424));
#18381=CARTESIAN_POINT('',(-0.037670271841,-0.021512272175,0.001528665498));
#18382=CARTESIAN_POINT('',(-0.037251993154,-0.021624404365,0.001417680399));
#18383=CARTESIAN_POINT('',(-0.03741046422,-0.021872807115,0.001753957271));
#18384=CARTESIAN_POINT('',(-0.037654725402,-0.021486538245,0.001553695464));
#18385=CARTESIAN_POINT('',(-0.037239813053,-0.021601592947,0.001443571051));
#18386=CARTESIAN_POINT('',(-0.037394917781,-0.021843465289,0.001782691183));
#18387=CARTESIAN_POINT('',(-0.037623119912,-0.02143432279,0.001602024868));
#18388=CARTESIAN_POINT('',(-0.037214887215,-0.021554976073,0.00149395412));
#18389=CARTESIAN_POINT('',(-0.037363312291,-0.021783929826,0.001838175481));
#18390=CARTESIAN_POINT('',(-0.037607024828,-0.021407781395,0.001625388759));
#18391=CARTESIAN_POINT('',(-0.037202122033,-0.021531133535,0.001518515298));
#18392=CARTESIAN_POINT('',(-0.037347217206,-0.021753667921,0.001864999845));
#18393=CARTESIAN_POINT('',(-0.037525118351,-0.02127298417,0.001738333831));
#18394=CARTESIAN_POINT('',(-0.037137549676,-0.021410705958,0.001636725622));
#18395=CARTESIAN_POINT('',(-0.03726531073,-0.02159997676,0.001994681424));
#18396=CARTESIAN_POINT('',(-0.037455051799,-0.02115851676,0.001816399876));
#18397=CARTESIAN_POINT('',(-0.037080651573,-0.021305121671,0.001722755165));
#18398=CARTESIAN_POINT('',(-0.037195244178,-0.021469469996,0.002084341855));
#18399=CARTESIAN_POINT('',(-0.037343235527,-0.020977588541,0.001916132313));
#18400=CARTESIAN_POINT('',(-0.036986748025,-0.021132256941,0.001837126924));
#18401=CARTESIAN_POINT('',(-0.037083427906,-0.021263200951,0.002198928626));
#18402=CARTESIAN_POINT('',(-0.03730475018,-0.020915593919,0.001946487158));
#18403=CARTESIAN_POINT('',(-0.03695443279,-0.021072974284,0.001872428345));
#18404=CARTESIAN_POINT('',(-0.037044942559,-0.021192525146,0.002233812936));
#18405=CARTESIAN_POINT('',(-0.03722687049,-0.020790753789,0.002000458179));
#18406=CARTESIAN_POINT('',(-0.036888415857,-0.020952363493,0.001936508103));
#18407=CARTESIAN_POINT('',(-0.036967062869,-0.021050207598,0.00229585445));
#18408=CARTESIAN_POINT('',(-0.037187320072,-0.020727654338,0.002024230796));
#18409=CARTESIAN_POINT('',(-0.036854627768,-0.020890866611,0.001965551201));
#18410=CARTESIAN_POINT('',(-0.036927512451,-0.020978276332,0.002323191356));
#18411=CARTESIAN_POINT('',(-0.03706685504,-0.020536431836,0.002086313851));
#18412=CARTESIAN_POINT('',(-0.036751742399,-0.020704420727,0.002042869105));
#18413=CARTESIAN_POINT('',(-0.036807047419,-0.020760295815,0.0023946124));
#18414=CARTESIAN_POINT('',(-0.03698413842,-0.020406401217,0.002115462885));
#18415=CARTESIAN_POINT('',(-0.036679594089,-0.020574684762,0.002083292386));
#18416=CARTESIAN_POINT('',(-0.036724330798,-0.020612078707,0.002428191144));
#18417=CARTESIAN_POINT('',(-0.036813690053,-0.020141406598,0.002149499788));
#18418=CARTESIAN_POINT('',(-0.036528822624,-0.020306284053,0.002138531962));
#18419=CARTESIAN_POINT('',(-0.036553882432,-0.020310043308,0.002467518924));
#18420=CARTESIAN_POINT('',(-0.03672806298,-0.020009717442,0.002153964617));
#18421=CARTESIAN_POINT('',(-0.036452219097,-0.020171139995,0.002153473299));
#18422=CARTESIAN_POINT('',(-0.036468255359,-0.020159957651,0.002472779113));
#18423=CARTESIAN_POINT('',(-0.036556082968,-0.019748156007,0.00213921308));
#18424=CARTESIAN_POINT('',(-0.036296957641,-0.019900051219,0.002157080292));
#18425=CARTESIAN_POINT('',(-0.036296275347,-0.019861881178,0.002456116136));
#18426=CARTESIAN_POINT('',(-0.036469700557,-0.019618238496,0.002119999249));
#18427=CARTESIAN_POINT('',(-0.036218299035,-0.019764020339,0.002146573084));
#18428=CARTESIAN_POINT('',(-0.03620989256,-0.019713838176,0.002434195848));
#18429=CARTESIAN_POINT('',(-0.0363829297,-0.019489230098,0.002088447775));
#18430=CARTESIAN_POINT('',(-0.036137554584,-0.019625886228,0.002121869649));
#18431=CARTESIAN_POINT('',(-0.036123122079,-0.019566845848,0.00239810651));
#18432=CARTESIAN_POINT('',(-0.0387712812776744,-1.75917835919922E-11,3.89705915929546E-17));
#18433=CARTESIAN_POINT('',(-0.0363829297,-0.011553263876,-0.015833944478));
#18434=CARTESIAN_POINT('',(-0.036137554584,-0.011650536133,-0.015935581221));
#18435=CARTESIAN_POINT('',(-0.036123122079,-0.011860244082,-0.015746332321));
#18436=CARTESIAN_POINT('',(-0.036296388628,-0.011461678478,-0.015738249755));
#18437=CARTESIAN_POINT('',(-0.036059352191,-0.01156292323,-0.015831682636));
#18438=CARTESIAN_POINT('',(-0.03603658062,-0.011755770109,-0.015637366271));
#18439=CARTESIAN_POINT('',(-0.036211750879,-0.011362340175,-0.015652006375));
#18440=CARTESIAN_POINT('',(-0.03598108599,-0.011464890175,-0.015735268277));
#18441=CARTESIAN_POINT('',(-0.035951943258,-0.011642376917,-0.015539235616));
#18442=CARTESIAN_POINT('',(-0.036046427611,-0.011148355448,-0.015498106242));
#18443=CARTESIAN_POINT('',(-0.03582764111,-0.011250375413,-0.0155622207));
#18444=CARTESIAN_POINT('',(-0.03578661999,-0.011397963715,-0.015364286119));
#18445=CARTESIAN_POINT('',(-0.035965731891,-0.011033717779,-0.015430430805));
#18446=CARTESIAN_POINT('',(-0.035752240428,-0.011134208806,-0.015484897869));
#18447=CARTESIAN_POINT('',(-0.03570592427,-0.011266954373,-0.015287446383));
#18448=CARTESIAN_POINT('',(-0.035867783855,-0.01087985013,-0.015358489273));
#18449=CARTESIAN_POINT('',(-0.035659677357,-0.010975190542,-0.015401223282));
#18450=CARTESIAN_POINT('',(-0.035607976234,-0.011091013549,-0.015205907441));
#18451=CARTESIAN_POINT('',(-0.03584830488,-0.010848477709,-0.015344716547));
#18452=CARTESIAN_POINT('',(-0.035641412325,-0.010942986155,-0.015385276872));
#18453=CARTESIAN_POINT('',(-0.035588497259,-0.011055135885,-0.015190305996));
#18454=CARTESIAN_POINT('',(-0.035810061793,-0.010785289725,-0.015318762179));
#18455=CARTESIAN_POINT('',(-0.035605524332,-0.010877986763,-0.015355106157));
#18456=CARTESIAN_POINT('',(-0.035550254172,-0.010982864209,-0.015160923786));
#18457=CARTESIAN_POINT('',(-0.035791254693,-0.010753409687,-0.015306546858));
#18458=CARTESIAN_POINT('',(-0.035587855191,-0.01084512498,-0.015340831622));
#18459=CARTESIAN_POINT('',(-0.035531447072,-0.01094639649,-0.015147104814));
#18460=CARTESIAN_POINT('',(-0.035735788251,-0.010656907808,-0.015272182929));
#18461=CARTESIAN_POINT('',(-0.035535852231,-0.010745740813,-0.015300591903));
#18462=CARTESIAN_POINT('',(-0.03547598063,-0.01083599326,-0.015108260194));
#18463=CARTESIAN_POINT('',(-0.035700081089,-0.010591426457,-0.015252310709));
#18464=CARTESIAN_POINT('',(-0.035502196601,-0.010677860391,-0.015276916375));
#18465=CARTESIAN_POINT('',(-0.035440273468,-0.010761060282,-0.015085840387));
#18466=CARTESIAN_POINT('',(-0.035596955729,-0.010391434585,-0.015201975242));
#18467=CARTESIAN_POINT('',(-0.035405412743,-0.010470970184,-0.015216375149));
#18468=CARTESIAN_POINT('',(-0.035337148108,-0.01053214264,-0.01502920465));
#18469=CARTESIAN_POINT('',(-0.035533471872,-0.010253427089,-0.015180668075));
#18470=CARTESIAN_POINT('',(-0.03534514464,-0.010326512046,-0.015188782336));
#18471=CARTESIAN_POINT('',(-0.035273664252,-0.010374098072,-0.015005469481));
#18472=CARTESIAN_POINT('',(-0.035462076716,-0.010074076964,-0.015171484429));
#18473=CARTESIAN_POINT('',(-0.035277056499,-0.010137100933,-0.015173629506));
#18474=CARTESIAN_POINT('',(-0.035202269094,-0.01016859868,-0.014995769339));
#18475=CARTESIAN_POINT('',(-0.035448157312,-0.010037740585,-0.015170531646));
#18476=CARTESIAN_POINT('',(-0.035263851039,-0.01009891748,-0.015171574453));
#18477=CARTESIAN_POINT('',(-0.035188349691,-0.010126959086,-0.014994841338));
#18478=CARTESIAN_POINT('',(-0.035421421576,-0.009964994461,-0.015170485375));
#18479=CARTESIAN_POINT('',(-0.035238481118,-0.010022418853,-0.015169521732));
#18480=CARTESIAN_POINT('',(-0.035161613954,-0.010043584805,-0.01499510979));
#18481=CARTESIAN_POINT('',(-0.035408615027,-0.009928623211,-0.015171384646));
#18482=CARTESIAN_POINT('',(-0.035226318844,-0.00998413467599999,-0.015169509426));
#18483=CARTESIAN_POINT('',(-0.035148807406,-0.010001894278,-0.014996297799));
#18484=CARTESIAN_POINT('',(-0.035371903227,-0.009819511029,-0.015176859697));
#18485=CARTESIAN_POINT('',(-0.035191509303,-0.009869419344,-0.015172544106));
#18486=CARTESIAN_POINT('',(-0.035112095605,-0.00987680808,-0.015003034244));
#18487=CARTESIAN_POINT('',(-0.035349701075,-0.009746771624,-0.015184204718));
#18488=CARTESIAN_POINT('',(-0.035170375015,-0.009792664461,-0.015178628799));
#18489=CARTESIAN_POINT('',(-0.035089893455,-0.009793397768,-0.015011745976));
#18490=CARTESIAN_POINT('',(-0.035310076825,-0.009601277538,-0.015206522019));
#18491=CARTESIAN_POINT('',(-0.035132682741,-0.009639118677,-0.015199261909));
#18492=CARTESIAN_POINT('',(-0.035050269204,-0.009626515241,-0.01503787977));
#18493=CARTESIAN_POINT('',(-0.035292653375,-0.00952852287,-0.015221492219));
#18494=CARTESIAN_POINT('',(-0.035116074086,-0.009562226397,-0.015213776324));
#18495=CARTESIAN_POINT('',(-0.035032845755,-0.009543043046,-0.015055299453));
#18496=CARTESIAN_POINT('',(-0.035270404132,-0.009419365813,-0.015250054381));
#18497=CARTESIAN_POINT('',(-0.035094864144,-0.009446800679,-0.015242325899));
#18498=CARTESIAN_POINT('',(-0.03501059651,-0.009417771664,-0.015088401097));
#18499=CARTESIAN_POINT('',(-0.03526362249,-0.009382869798,-0.015260634503));
#18500=CARTESIAN_POINT('',(-0.035088401673,-0.009408236182,-0.01525299799));
#18501=CARTESIAN_POINT('',(-0.035003814869,-0.009375882126,-0.015100644955));
#18502=CARTESIAN_POINT('',(-0.035251577427,-0.009310843156,-0.015283600698));
#18503=CARTESIAN_POINT('',(-0.035076925826,-0.00933214641500001,-0.015276357005));
#18504=CARTESIAN_POINT('',(-0.034991769806,-0.009293199654,-0.015127189761));
#18505=CARTESIAN_POINT('',(-0.035246291308,-0.009275220092,-0.015296004916));
#18506=CARTESIAN_POINT('',(-0.035071886429,-0.009294507868,-0.015289062514));
#18507=CARTESIAN_POINT('',(-0.034986483687,-0.009252300671,-0.015141511843));
#18508=CARTESIAN_POINT('',(-0.035223521483,-0.009099035104,-0.015362584279));
#18509=CARTESIAN_POINT('',(-0.035050225188,-0.00910877567300001,-0.01535752223));
#18510=CARTESIAN_POINT('',(-0.034963713862,-0.009049994038,-0.015218315908));
#18511=CARTESIAN_POINT('',(-0.035216913712,-0.008964197582,-0.015430279341));
#18512=CARTESIAN_POINT('',(-0.035043883179,-0.008966030964,-0.01542863008));
#18513=CARTESIAN_POINT('',(-0.034957106091,-0.008895075333,-0.015296202211));
#18514=CARTESIAN_POINT('',(-0.035223876434,-0.00880361429,-0.015533717464));
#18515=CARTESIAN_POINT('',(-0.035050518048,-0.008797299153,-0.015537902482));
#18516=CARTESIAN_POINT('',(-0.034964068813,-0.008710470427,-0.015414991225));
#18517=CARTESIAN_POINT('',(-0.03522604562,-0.008771889308,-0.015555375611));
#18518=CARTESIAN_POINT('',(-0.035052587043,-0.008763972426,-0.01556084085));
#18519=CARTESIAN_POINT('',(-0.034966237999,-0.008673994043,-0.015439854351));
#18520=CARTESIAN_POINT('',(-0.035231850552,-0.008710185979,-0.01559994762));
#18521=CARTESIAN_POINT('',(-0.035058120997,-0.008699242413,-0.015608106609));
#18522=CARTESIAN_POINT('',(-0.034972042931,-0.008603038604,-0.015491004502));
#18523=CARTESIAN_POINT('',(-0.0352354894,-0.008680084706,-0.015622937235));
#18524=CARTESIAN_POINT('',(-0.035061591095,-0.008667698117,-0.015632524608));
#18525=CARTESIAN_POINT('',(-0.034975681779,-0.008568418251,-0.01551737855));
#18526=CARTESIAN_POINT('',(-0.035248550352,-0.008591972563,-0.015693962252));
#18527=CARTESIAN_POINT('',(-0.035074046816,-0.008575454015,-0.015708073142));
#18528=CARTESIAN_POINT('',(-0.034988742731,-0.008467061961,-0.015598835312));
#18529=CARTESIAN_POINT('',(-0.035260111701,-0.008536147393,-0.015744048097));
#18530=CARTESIAN_POINT('',(-0.035085080525,-0.008517189165,-0.015761475243));
#18531=CARTESIAN_POINT('',(-0.03500030408,-0.008402823979,-0.015656246123));
#18532=CARTESIAN_POINT('',(-0.035281577861,-0.008456663156,-0.015823174106));
#18533=CARTESIAN_POINT('',(-0.035105505104,-0.008434683838,-0.015845779289));
#18534=CARTESIAN_POINT('',(-0.03502177024,-0.00831133067,-0.015746900341));
#18535=CARTESIAN_POINT('',(-0.035289421938,-0.008430878868,-0.015850217121));
#18536=CARTESIAN_POINT('',(-0.035112977015,-0.008407947185,-0.015874642529));
#18537=CARTESIAN_POINT('',(-0.035029614317,-0.008281645265,-0.015777876425));
#18538=CARTESIAN_POINT('',(-0.035306476701,-0.008380728899,-0.015905637862));
#18539=CARTESIAN_POINT('',(-0.035129211644,-0.008356075565,-0.015933800795));
#18540=CARTESIAN_POINT('',(-0.03504666908,-0.008223896938,-0.015841343859));
#18541=CARTESIAN_POINT('',(-0.035315718145,-0.008356292952,-0.015934104044));
#18542=CARTESIAN_POINT('',(-0.035138009535,-0.00833086275400001,-0.015964204293));
#18543=CARTESIAN_POINT('',(-0.035055910524,-0.008195753062,-0.015873936458));
#18544=CARTESIAN_POINT('',(-0.035345244257,-0.008285697845,-0.016020806527));
#18545=CARTESIAN_POINT('',(-0.035166136457,-0.00825813904900001,-0.01605692694));
#18546=CARTESIAN_POINT('',(-0.035085436637,-0.008114429329,-0.015973187908));
#18547=CARTESIAN_POINT('',(-0.035367258146,-0.008242329816,-0.016080187826));
#18548=CARTESIAN_POINT('',(-0.035187092355,-0.008213803598,-0.016120416082));
#18549=CARTESIAN_POINT('',(-0.035107450524,-0.008064447951,-0.016041138718));
#18550=CARTESIAN_POINT('',(-0.035415540032,-0.008162463636,-0.016201911227));
#18551=CARTESIAN_POINT('',(-0.035232955499,-0.008132780528,-0.016250421064));
#18552=CARTESIAN_POINT('',(-0.035155732411,-0.007972359488,-0.016180383385));
#18553=CARTESIAN_POINT('',(-0.035441809443,-0.008125967618,-0.016264254219));
#18554=CARTESIAN_POINT('',(-0.035257918294,-0.008096097371,-0.016317036983));
#18555=CARTESIAN_POINT('',(-0.035182001822,-0.007930254845,-0.016251678255));
#18556=CARTESIAN_POINT('',(-0.035498359317,-0.008059587534,-0.016391815963));
#18557=CARTESIAN_POINT('',(-0.035311533473,-0.00803010615599999,-0.016453125142));
#18558=CARTESIAN_POINT('',(-0.035238551696,-0.007853625833,-0.016397516267));
#18559=CARTESIAN_POINT('',(-0.035528803299,-0.008029593217,-0.016457359612));
#18560=CARTESIAN_POINT('',(-0.035340397738,-0.008000717817,-0.016523037284));
#18561=CARTESIAN_POINT('',(-0.035268995678,-0.007818973813,-0.016472430579));
#18562=CARTESIAN_POINT('',(-0.035624302868,-0.007950706059,-0.016654920378));
#18563=CARTESIAN_POINT('',(-0.035431143853,-0.00792437715800001,-0.016734311632));
#18564=CARTESIAN_POINT('',(-0.035364495247,-0.007727753242,-0.016698182027));
#18565=CARTESIAN_POINT('',(-0.035693625065,-0.00791237942,-0.016788320669));
#18566=CARTESIAN_POINT('',(-0.035496770299,-0.00788970285099999,-0.016876219964));
#18567=CARTESIAN_POINT('',(-0.035433817443,-0.007683310981,-0.016850547386));
#18568=CARTESIAN_POINT('',(-0.035804878296,-0.007874305366,-0.016990897542));
#18569=CARTESIAN_POINT('',(-0.035600812464,-0.007858960081,-0.01708919141));
#18570=CARTESIAN_POINT('',(-0.035545070675,-0.0076389311,-0.017081837817));
#18571=CARTESIAN_POINT('',(-0.035843360668,-0.007864862098,-0.01705913467));
#18572=CARTESIAN_POINT('',(-0.035636958249,-0.007852300237,-0.017161183879));
#18573=CARTESIAN_POINT('',(-0.035583553047,-0.007627864561,-0.017159732511));
#18574=CARTESIAN_POINT('',(-0.035921655233,-0.007852607539,-0.017194668761));
#18575=CARTESIAN_POINT('',(-0.035710302083,-0.00784612017,-0.017303741424));
#18576=CARTESIAN_POINT('',(-0.035661847612,-0.007613348096,-0.017314422362));
#18577=CARTESIAN_POINT('',(-0.035961464931,-0.007849756022,-0.017261981032));
#18578=CARTESIAN_POINT('',(-0.035747535996,-0.00784663784700001,-0.017374356859));
#18579=CARTESIAN_POINT('',(-0.035701657309,-0.007609851942,-0.017391235154));
#18580=CARTESIAN_POINT('',(-0.036082708725,-0.007850536771,-0.017462656398));
#18581=CARTESIAN_POINT('',(-0.035861344783,-0.007858260977,-0.017585519353));
#18582=CARTESIAN_POINT('',(-0.035822901104,-0.007610083132,-0.017620198615));
#18583=CARTESIAN_POINT('',(-0.036165937985,-0.007863426326,-0.017594770655));
#18584=CARTESIAN_POINT('',(-0.035938765603,-0.00787975504899999,-0.017722847129));
#18585=CARTESIAN_POINT('',(-0.035906130364,-0.007624440672,-0.017770889103));
#18586=CARTESIAN_POINT('',(-0.036272749616,-0.007894708486,-0.017757945878));
#18587=CARTESIAN_POINT('',(-0.036036325391,-0.007921955923,-0.017889160917));
#18588=CARTESIAN_POINT('',(-0.036012941995,-0.007659800659,-0.017956955579));
#18589=CARTESIAN_POINT('',(-0.036294271622,-0.007901739857,-0.017790509137));
#18590=CARTESIAN_POINT('',(-0.036056160144,-0.00793132121100001,-0.017922622722));
#18591=CARTESIAN_POINT('',(-0.036034464001,-0.007667762066,-0.017994084324));
#18592=CARTESIAN_POINT('',(-0.036337241164,-0.007917210124,-0.017854907701));
#18593=CARTESIAN_POINT('',(-0.036095695252,-0.007951508517,-0.01798864385));
#18594=CARTESIAN_POINT('',(-0.036077433543,-0.007685302077,-0.018067506581));
#18595=CARTESIAN_POINT('',(-0.036358730845,-0.007925659835,-0.017886808044));
#18596=CARTESIAN_POINT('',(-0.03611543566,-0.007962357198,-0.018021267296));
#18597=CARTESIAN_POINT('',(-0.036098923223,-0.00769489288,-0.018103874262));
#18598=CARTESIAN_POINT('',(-0.036423211553,-0.007953112573,-0.017981630573));
#18599=CARTESIAN_POINT('',(-0.036174782484,-0.007997207555,-0.018118355391));
#18600=CARTESIAN_POINT('',(-0.036163403931,-0.00772608128,-0.018211968175));
#18601=CARTESIAN_POINT('',(-0.036466213928,-0.007974214849,-0.018043676239));
#18602=CARTESIAN_POINT('',(-0.036214084658,-0.008023322943,-0.01818130788));
#18603=CARTESIAN_POINT('',(-0.036206406307,-0.007750089872,-0.018282687553));
#18604=CARTESIAN_POINT('',(-0.036595254777,-0.008045769879,-0.018226375241));
#18605=CARTESIAN_POINT('',(-0.03633245937,-0.008110685029,-0.018367068303));
#18606=CARTESIAN_POINT('',(-0.036335447156,-0.007831586332,-0.018490897658));
#18607=CARTESIAN_POINT('',(-0.036681322249,-0.008104401696,-0.018343621837));
#18608=CARTESIAN_POINT('',(-0.036410235723,-0.00818013428299999,-0.018483802691));
#18609=CARTESIAN_POINT('',(-0.036421514628,-0.007898465521,-0.018624476296));
#18610=CARTESIAN_POINT('',(-0.03678899075,-0.008191880004,-0.01848425171));
#18611=CARTESIAN_POINT('',(-0.036505370032,-0.008279350682,-0.018620167377));
#18612=CARTESIAN_POINT('',(-0.036529183129,-0.007998347907,-0.018784644787));
#18613=CARTESIAN_POINT('',(-0.036810556304,-0.008210117449,-0.01851211236));
#18614=CARTESIAN_POINT('',(-0.036524605066,-0.00830017876800001,-0.018647392468));
#18615=CARTESIAN_POINT('',(-0.036550748683,-0.00801917556,-0.018816373614));
#18616=CARTESIAN_POINT('',(-0.036853337272,-0.008247729637,-0.018566762019));
#18617=CARTESIAN_POINT('',(-0.036562661331,-0.00834289234,-0.018700571843));
#18618=CARTESIAN_POINT('',(-0.036593529651,-0.008062137607,-0.018878605442));
#18619=CARTESIAN_POINT('',(-0.036874593816,-0.008267135902,-0.018593605562));
#18620=CARTESIAN_POINT('',(-0.036581516731,-0.008364823662,-0.018726570453));
#18621=CARTESIAN_POINT('',(-0.036614786195,-0.008084307983,-0.018909170561));
#18622=CARTESIAN_POINT('',(-0.036937968442,-0.00832714152,-0.018672700842));
#18623=CARTESIAN_POINT('',(-0.03663781018,-0.008432559434,-0.018803151489));
#18624=CARTESIAN_POINT('',(-0.03667816082,-0.008152871175,-0.01899922333));
#18625=CARTESIAN_POINT('',(-0.03697969206,-0.008369524049,-0.018723520226));
#18626=CARTESIAN_POINT('',(-0.036674489896,-0.008479793224,-0.018851625693));
#18627=CARTESIAN_POINT('',(-0.036719884461,-0.00820131189,-0.019057071854));
#18628=CARTESIAN_POINT('',(-0.037020900622,-0.008414292884,-0.018772414733));
#18629=CARTESIAN_POINT('',(-0.036710197303,-0.008528746736,-0.01889741608));
#18630=CARTESIAN_POINT('',(-0.036761093001,-0.008252492416,-0.019112717618));
#18631=CARTESIAN_POINT('',(-0.0370209006225329,-0.00819303142614902,-0.0189750063603988));
#18632=CARTESIAN_POINT('',(-0.036382929700134,-0.0117699983702051,-0.0156265169988628));
#18633=CARTESIAN_POINT('',(-0.0370209006725265,-0.00841429293889186,-0.0187724147929504));
#18634=CARTESIAN_POINT('',(-0.0367101973471479,-0.00852874679652509,-0.0188974161366143));
#18635=CARTESIAN_POINT('',(-0.0367610930515268,-0.00825249247875368,-0.0191127176862286));
#18636=CARTESIAN_POINT('',(-0.037103317012847,-0.00850382975946811,-0.0188702028728446));
#18637=CARTESIAN_POINT('',(-0.0367834353017993,-0.00862915328424695,-0.0189913348642332));
#18638=CARTESIAN_POINT('',(-0.0368435097848469,-0.00835485310428282,-0.0192240087409122));
#18639=CARTESIAN_POINT('',(-0.0371836845969985,-0.00860284405433526,-0.018960351265708));
#18640=CARTESIAN_POINT('',(-0.036852619292111,-0.00873678178590861,-0.0190740421504255));
#18641=CARTESIAN_POINT('',(-0.0369238769759985,-0.0084680943925531,-0.0193265564529946));
#18642=CARTESIAN_POINT('',(-0.037301116085,-0.008766788714,-0.019082991418));
#18643=CARTESIAN_POINT('',(-0.03695137278,-0.00890933196000001,-0.019182696761));
#18644=CARTESIAN_POINT('',(-0.037041308464,-0.008655658553,-0.019465980183));
#18645=CARTESIAN_POINT('',(-0.037339424126,-0.008823609321,-0.019121421839));
#18646=CARTESIAN_POINT('',(-0.036983551057,-0.00896908235600001,-0.019216348303));
#18647=CARTESIAN_POINT('',(-0.037079616505,-0.008720674816,-0.019509653949));
#18648=CARTESIAN_POINT('',(-0.037413681214,-0.008940547851,-0.01919260491));
#18649=CARTESIAN_POINT('',(-0.037045412802,-0.00909076204500001,-0.019277559802));
#18650=CARTESIAN_POINT('',(-0.037153873593,-0.00885449785,-0.019590514456));
#18651=CARTESIAN_POINT('',(-0.037449744946,-0.00900082422,-0.019225478294));
#18652=CARTESIAN_POINT('',(-0.037075133644,-0.009152864878,-0.019305105559));
#18653=CARTESIAN_POINT('',(-0.037189937325,-0.008923485888,-0.019627838465));
#18654=CARTESIAN_POINT('',(-0.037519742735,-0.009125063699,-0.01928564172));
#18655=CARTESIAN_POINT('',(-0.037132298021,-0.00927948707199999,-0.019354318908));
#18656=CARTESIAN_POINT('',(-0.037259935114,-0.009065697806,-0.019696105522));
#18657=CARTESIAN_POINT('',(-0.037553677068,-0.009189026182,-0.019312932788));
#18658=CARTESIAN_POINT('',(-0.037159681014,-0.00934400000800001,-0.019375867489));
#18659=CARTESIAN_POINT('',(-0.037293869447,-0.009138920963,-0.019727049749));
#18660=CARTESIAN_POINT('',(-0.037602938649,-0.009287868388,-0.019349449243));
#18661=CARTESIAN_POINT('',(-0.037198872381,-0.009442158226,-0.01940357468));
#18662=CARTESIAN_POINT('',(-0.037343131027,-0.009252085639,-0.019768414058));
#18663=CARTESIAN_POINT('',(-0.037619085386,-0.009321299752,-0.01936088333));
#18664=CARTESIAN_POINT('',(-0.037211691522,-0.009475309863,-0.0194120754));
#18665=CARTESIAN_POINT('',(-0.037359277765,-0.009290363203,-0.019781358588));
#18666=CARTESIAN_POINT('',(-0.037650817756,-0.009389164887,-0.019382217481));
#18667=CARTESIAN_POINT('',(-0.037236742776,-0.009542219848,-0.019427532009));
#18668=CARTESIAN_POINT('',(-0.037391010135,-0.00936806994,-0.019805494239));
#18669=CARTESIAN_POINT('',(-0.037666411882,-0.009423626067,-0.019392118348));
#18670=CARTESIAN_POINT('',(-0.037248972401,-0.00957599822699999,-0.019434471815));
#18671=CARTESIAN_POINT('',(-0.037406604261,-0.009407530512,-0.019816686195));
#18672=CARTESIAN_POINT('',(-0.037742059103,-0.009596469576,-0.019437127945));
#18673=CARTESIAN_POINT('',(-0.037308672836,-0.009746481892,-0.019465277981));
#18674=CARTESIAN_POINT('',(-0.037482251481,-0.009605458605,-0.0198675155));
#18675=CARTESIAN_POINT('',(-0.037795953594,-0.009737990873,-0.019459408654));
#18676=CARTESIAN_POINT('',(-0.037349209561,-0.00988085362499999,-0.019475955808));
#18677=CARTESIAN_POINT('',(-0.037536145973,-0.009767548722,-0.019892505579));
#18678=CARTESIAN_POINT('',(-0.037866774638,-0.00995526822,-0.019471266124));
#18679=CARTESIAN_POINT('',(-0.037401307565,-0.010081722694,-0.019473703662));
#18680=CARTESIAN_POINT('',(-0.037606967016,-0.010016452968,-0.019905364135));
#18681=CARTESIAN_POINT('',(-0.037888699602,-0.010028532389,-0.019471600233));
#18682=CARTESIAN_POINT('',(-0.037417279271,-0.010149079247,-0.019469741824));
#18683=CARTESIAN_POINT('',(-0.037628891981,-0.010100389312,-0.019905517967));
#18684=CARTESIAN_POINT('',(-0.037918925522,-0.010139765166,-0.0194662815));
#18685=CARTESIAN_POINT('',(-0.037439020962,-0.010250061616,-0.019459037412));
#18686=CARTESIAN_POINT('',(-0.037659117901,-0.010227838031,-0.01989910134));
#18687=CARTESIAN_POINT('',(-0.037928582819,-0.010177183975,-0.019463520333));
#18688=CARTESIAN_POINT('',(-0.037445936687,-0.010283943964,-0.019454625919));
#18689=CARTESIAN_POINT('',(-0.037668775198,-0.010270714068,-0.019895833342));
#18690=CARTESIAN_POINT('',(-0.037946745879,-0.010251529703,-0.019456070883));
#18691=CARTESIAN_POINT('',(-0.0374588757169999,-0.010350958591,-0.019444295419));
#18692=CARTESIAN_POINT('',(-0.037686938258,-0.01035590701,-0.019887098991));
#18693=CARTESIAN_POINT('',(-0.03795527555,-0.010288532493,-0.019451385246));
#18694=CARTESIAN_POINT('',(-0.037464908394,-0.010384139251,-0.019438369006));
#18695=CARTESIAN_POINT('',(-0.037695467929,-0.010398310834,-0.019881635422));
#18696=CARTESIAN_POINT('',(-0.037995201404,-0.0104727007,-0.019423189771));
#18697=CARTESIAN_POINT('',(-0.037493219634,-0.010549838583,-0.019404818528));
#18698=CARTESIAN_POINT('',(-0.037735393783,-0.010609372239,-0.01984887779));
#18699=CARTESIAN_POINT('',(-0.03801852767,-0.010617356474,-0.019385538099));
#18700=CARTESIAN_POINT('',(-0.037508976952,-0.010676036879,-0.019366609516));
#18701=CARTESIAN_POINT('',(-0.037758720049,-0.010775187757,-0.01980544701));
#18702=CARTESIAN_POINT('',(-0.038040144091,-0.010830087113,-0.019305249844));
#18703=CARTESIAN_POINT('',(-0.037523624808,-0.010861368197,-0.019291823728));
#18704=CARTESIAN_POINT('',(-0.03778033647,-0.011019102134,-0.019713124546));
#18705=CARTESIAN_POINT('',(-0.038045091154,-0.010900659463,-0.01927424932));
#18706=CARTESIAN_POINT('',(-0.037526947936,-0.010922751921,-0.019263695619));
#18707=CARTESIAN_POINT('',(-0.037785283533,-0.011100031176,-0.01967751236));
#18708=CARTESIAN_POINT('',(-0.038050108278,-0.011036551943,-0.019205674484));
#18709=CARTESIAN_POINT('',(-0.037530327064,-0.011041355675,-0.019202654737));
#18710=CARTESIAN_POINT('',(-0.037790300657,-0.011255891492,-0.01959879628));
#18711=CARTESIAN_POINT('',(-0.038050243047,-0.011102269591,-0.019167998017));
#18712=CARTESIAN_POINT('',(-0.037530417095,-0.011098746343,-0.01916971836));
#18713=CARTESIAN_POINT('',(-0.037790435426,-0.011331278423,-0.019555574534));
#18714=CARTESIAN_POINT('',(-0.038045857381,-0.011229333988,-0.019085998172));
#18715=CARTESIAN_POINT('',(-0.037527464034,-0.011210579299,-0.019098653928));
#18716=CARTESIAN_POINT('',(-0.03778604976,-0.011477065914,-0.019461552266));
#18717=CARTESIAN_POINT('',(-0.038041336883,-0.011290680666,-0.019041674687));
#18718=CARTESIAN_POINT('',(-0.037524429559,-0.011264860653,-0.019060637682));
#18719=CARTESIAN_POINT('',(-0.037781529262,-0.011547466388,-0.019410751623));
#18720=CARTESIAN_POINT('',(-0.038027559938,-0.011408940944,-0.018946286813));
#18721=CARTESIAN_POINT('',(-0.037515080889,-0.011370775304,-0.018978926179));
#18722=CARTESIAN_POINT('',(-0.037767752317,-0.011683211699,-0.019301463566));
#18723=CARTESIAN_POINT('',(-0.038018235775,-0.011465994202,-0.018895009009));
#18724=CARTESIAN_POINT('',(-0.037508746133,-0.011422411288,-0.018935184096));
#18725=CARTESIAN_POINT('',(-0.037758428154,-0.011748717175,-0.019242731993));
#18726=CARTESIAN_POINT('',(-0.037983863425,-0.011626135813,-0.018735057854));
#18727=CARTESIAN_POINT('',(-0.037485152239,-0.011569149469,-0.018798617961));
#18728=CARTESIAN_POINT('',(-0.037724055805,-0.011932636702,-0.01905958005));
#18729=CARTESIAN_POINT('',(-0.03795238138,-0.011719875549,-0.018619223276));
#18730=CARTESIAN_POINT('',(-0.037463427014,-0.011658126499,-0.018699531784));
#18731=CARTESIAN_POINT('',(-0.037692573758,-0.012040369285,-0.018927005758));
#18732=CARTESIAN_POINT('',(-0.037902538675,-0.01182142833,-0.018463435089));
#18733=CARTESIAN_POINT('',(-0.037427207905,-0.011759803085,-0.018561524169));
#18734=CARTESIAN_POINT('',(-0.037642731053,-0.012157190014,-0.018748770563));
#18735=CARTESIAN_POINT('',(-0.0378920119,-0.011840990207,-0.018431644379));
#18736=CARTESIAN_POINT('',(-0.037419583631,-0.011779451696,-0.018533495969));
#18737=CARTESIAN_POINT('',(-0.037632204279,-0.012179699312,-0.018712402395));
#18738=CARTESIAN_POINT('',(-0.037870126119,-0.011878130234,-0.018367644958));
#18739=CARTESIAN_POINT('',(-0.037403612981,-0.011817220648,-0.018476768706));
#18740=CARTESIAN_POINT('',(-0.037610318498,-0.012222448524,-0.018639193956));
#18741=CARTESIAN_POINT('',(-0.037858748966,-0.011895754219,-0.018335374301));
#18742=CARTESIAN_POINT('',(-0.037395262434,-0.011835384713,-0.018448035028));
#18743=CARTESIAN_POINT('',(-0.037598941345,-0.012242741131,-0.018602282796));
#18744=CARTESIAN_POINT('',(-0.037823348421,-0.011945883489,-0.018237779846));
#18745=CARTESIAN_POINT('',(-0.037369172913,-0.011887572482,-0.018360946022));
#18746=CARTESIAN_POINT('',(-0.0375635408,-0.012300482293,-0.018490662919));
#18747=CARTESIAN_POINT('',(-0.037798059306,-0.011975653238,-0.018171675593));
#18748=CARTESIAN_POINT('',(-0.037350277137,-0.011919662954,-0.018301226609));
#18749=CARTESIAN_POINT('',(-0.037538251684,-0.012334802364,-0.01841507009));
#18750=CARTESIAN_POINT('',(-0.037744193093,-0.012028207852,-0.018037491178));
#18751=CARTESIAN_POINT('',(-0.037309379895,-0.011978153369,-0.018178502137));
#18752=CARTESIAN_POINT('',(-0.037484385472,-0.012395455267,-0.018261646389));
#18753=CARTESIAN_POINT('',(-0.037715615604,-0.012050991651,-0.017969410681));
#18754=CARTESIAN_POINT('',(-0.037287455068,-0.012004589867,-0.018115639729));
#18755=CARTESIAN_POINT('',(-0.037455807983,-0.012421786873,-0.018183815137));
#18756=CARTESIAN_POINT('',(-0.037670271841,-0.012079999243,-0.017865841447));
#18757=CARTESIAN_POINT('',(-0.037251993154,-0.012039949422,-0.018018443323));
#18758=CARTESIAN_POINT('',(-0.03741046422,-0.012455375111,-0.018065427979));
#18759=CARTESIAN_POINT('',(-0.037654725402,-0.012088808864,-0.017831040227));
#18760=CARTESIAN_POINT('',(-0.037239813053,-0.012050965676,-0.017985742729));
#18761=CARTESIAN_POINT('',(-0.037394917781,-0.012465588496,-0.018025650255));
#18762=CARTESIAN_POINT('',(-0.037623119912,-0.012104555629,-0.017761655615));
#18763=CARTESIAN_POINT('',(-0.037214887215,-0.012071290256,-0.017920179797));
#18764=CARTESIAN_POINT('',(-0.037363312291,-0.012483871576,-0.017946348883));
#18765=CARTESIAN_POINT('',(-0.037607024828,-0.012111518654,-0.017726988147));
#18766=CARTESIAN_POINT('',(-0.037202122033,-0.012080639592,-0.017887250964));
#18767=CARTESIAN_POINT('',(-0.037347217206,-0.012491971204,-0.017906729123));
#18768=CARTESIAN_POINT('',(-0.037525118351,-0.012141933343,-0.01755377779));
#18769=CARTESIAN_POINT('',(-0.037137549676,-0.012122798947,-0.017723852461));
#18770=CARTESIAN_POINT('',(-0.03726531073,-0.012527433166,-0.017708787883));
#18771=CARTESIAN_POINT('',(-0.037455051799,-0.012152306816,-0.017415613082));
#18772=CARTESIAN_POINT('',(-0.037080651573,-0.012144510573,-0.017589399015));
#18773=CARTESIAN_POINT('',(-0.037195244178,-0.012539827994,-0.017550935495));
#18774=CARTESIAN_POINT('',(-0.037343235527,-0.012148213531,-0.01720905843));
#18775=CARTESIAN_POINT('',(-0.036986748025,-0.012157127057,-0.017382507888));
#18776=CARTESIAN_POINT('',(-0.037083427906,-0.012535928527,-0.017315007876));
#18777=CARTESIAN_POINT('',(-0.03730475018,-0.012143504287,-0.01714019209));
#18778=CARTESIAN_POINT('',(-0.03695443279,-0.012158057656,-0.017313516891));
#18779=CARTESIAN_POINT('',(-0.037044942559,-0.012530801323,-0.017236358679));
#18780=CARTESIAN_POINT('',(-0.03722687049,-0.012127824497,-0.017005091856));
#18781=CARTESIAN_POINT('',(-0.036888415857,-0.012153246959,-0.017177025003));
#18782=CARTESIAN_POINT('',(-0.036967062869,-0.012513372076,-0.01708208731));
#18783=CARTESIAN_POINT('',(-0.037187320072,-0.012116862461,-0.016938559819));
#18784=CARTESIAN_POINT('',(-0.036854627768,-0.012147650578,-0.017109245591));
#18785=CARTESIAN_POINT('',(-0.036927512451,-0.012501080898,-0.017006124553));
#18786=CARTESIAN_POINT('',(-0.03706685504,-0.012075016713,-0.016741914748));
#18787=CARTESIAN_POINT('',(-0.036751742399,-0.012121386905,-0.016909119768));
#18788=CARTESIAN_POINT('',(-0.036807047419,-0.012453943078,-0.016781637365));
#18789=CARTESIAN_POINT('',(-0.03698413842,-0.012035245207,-0.016614730411));
#18790=CARTESIAN_POINT('',(-0.036679594089,-0.012091526511,-0.016776553485));
#18791=CARTESIAN_POINT('',(-0.036724330798,-0.01240891457,-0.016636488213));
#18792=CARTESIAN_POINT('',(-0.036813690053,-0.011932224721,-0.016368219888));
#18793=CARTESIAN_POINT('',(-0.036528822624,-0.012005165032,-0.016516491866));
#18794=CARTESIAN_POINT('',(-0.036553882432,-0.012291955726,-0.016355253995));
#18795=CARTESIAN_POINT('',(-0.03672806298,-0.011870246798,-0.016251941319));
#18796=CARTESIAN_POINT('',(-0.036452219097,-0.011950532581,-0.016391983009));
#18797=CARTESIAN_POINT('',(-0.036468255359,-0.012221468356,-0.016222645908));
#18798=CARTESIAN_POINT('',(-0.036556082968,-0.011726690875,-0.01603279824));
#18799=CARTESIAN_POINT('',(-0.036296957641,-0.01181811194,-0.016155409747));
#18800=CARTESIAN_POINT('',(-0.036296275347,-0.012057999557,-0.015972835599));
#18801=CARTESIAN_POINT('',(-0.036469700557,-0.011645092454,-0.01592989329));
#18802=CARTESIAN_POINT('',(-0.036218299035,-0.011740996991,-0.016042857153));
#18803=CARTESIAN_POINT('',(-0.03620989256,-0.011964994531,-0.015855586742));
#18804=CARTESIAN_POINT('',(-0.0363829297,-0.011553263876,-0.015833944478));
#18805=CARTESIAN_POINT('',(-0.036137554584,-0.011650536133,-0.015935581221));
#18806=CARTESIAN_POINT('',(-0.036123122079,-0.011860244082,-0.015746332321));
#18807=CARTESIAN_POINT('',(-0.0387712812904532,-1.29150202956894E-11,-1.90102621199567E-11));
#18808=CARTESIAN_POINT('',(0.0175000000000004,-0.0175000000000004,1.10617214860196E-34));
#18809=MECHANICAL_DESIGN_GEOMETRIC_PRESENTATION_REPRESENTATION('',(#8174,
#8175,#8176,#8177,#8178,#8179),#18810);
#18810=(
GEOMETRIC_REPRESENTATION_CONTEXT(3)
GLOBAL_UNCERTAINTY_ASSIGNED_CONTEXT((#18817))
GLOBAL_UNIT_ASSIGNED_CONTEXT((#18826,#18825,#18824))
REPRESENTATION_CONTEXT('MAS-697','TOP_LEVEL_ASSEMBLY_PART')
);
#18811=(
GEOMETRIC_REPRESENTATION_CONTEXT(3)
GLOBAL_UNCERTAINTY_ASSIGNED_CONTEXT((#18818))
GLOBAL_UNIT_ASSIGNED_CONTEXT((#18826,#18825,#18824))
REPRESENTATION_CONTEXT('cassette body__ DE    15749','COMPONENT_PART')
);
#18812=(
GEOMETRIC_REPRESENTATION_CONTEXT(3)
GLOBAL_UNCERTAINTY_ASSIGNED_CONTEXT((#18819))
GLOBAL_UNIT_ASSIGNED_CONTEXT((#18826,#18825,#18824))
REPRESENTATION_CONTEXT('endcap2__ DE    22113','COMPONENT_PART')
);
#18813=(
GEOMETRIC_REPRESENTATION_CONTEXT(3)
GLOBAL_UNCERTAINTY_ASSIGNED_CONTEXT((#18820))
GLOBAL_UNIT_ASSIGNED_CONTEXT((#18826,#18825,#18824))
REPRESENTATION_CONTEXT('endcap__ DE    14671','COMPONENT_PART')
);
#18814=(
GEOMETRIC_REPRESENTATION_CONTEXT(3)
GLOBAL_UNCERTAINTY_ASSIGNED_CONTEXT((#18821))
GLOBAL_UNIT_ASSIGNED_CONTEXT((#18826,#18825,#18824))
REPRESENTATION_CONTEXT(
'angular contact ball bearing_68_bsi_BS 6267 ABB - 4815 - 18,SI,NC,18_
68__ DE    23193','COMPONENT_PART')
);
#18815=(
GEOMETRIC_REPRESENTATION_CONTEXT(3)
GLOBAL_UNCERTAINTY_ASSIGNED_CONTEXT((#18822))
GLOBAL_UNIT_ASSIGNED_CONTEXT((#18826,#18825,#18824))
REPRESENTATION_CONTEXT(
'angular contact ball bearing_68_bsi_BS 6267 ABB - 4815 - 18,SI,NC,18_
68__ DE    23193','COMPONENT_PART')
);
#18816=(
GEOMETRIC_REPRESENTATION_CONTEXT(3)
GLOBAL_UNCERTAINTY_ASSIGNED_CONTEXT((#18823))
GLOBAL_UNIT_ASSIGNED_CONTEXT((#18826,#18825,#18824))
REPRESENTATION_CONTEXT('HubBody__ DE       35','COMPONENT_PART')
);
#18817=UNCERTAINTY_MEASURE_WITH_UNIT(LENGTH_MEASURE(1.E-8),#18826,
'DISTANCE_ACCURACY_VALUE','Maximum Tolerance applied to model');
#18818=UNCERTAINTY_MEASURE_WITH_UNIT(LENGTH_MEASURE(2.E-5),#18826,
'DISTANCE_ACCURACY_VALUE','Maximum Tolerance applied to model');
#18819=UNCERTAINTY_MEASURE_WITH_UNIT(LENGTH_MEASURE(2.E-5),#18826,
'DISTANCE_ACCURACY_VALUE','Maximum Tolerance applied to model');
#18820=UNCERTAINTY_MEASURE_WITH_UNIT(LENGTH_MEASURE(2.E-5),#18826,
'DISTANCE_ACCURACY_VALUE','Maximum Tolerance applied to model');
#18821=UNCERTAINTY_MEASURE_WITH_UNIT(LENGTH_MEASURE(2.E-5),#18826,
'DISTANCE_ACCURACY_VALUE','Maximum Tolerance applied to model');
#18822=UNCERTAINTY_MEASURE_WITH_UNIT(LENGTH_MEASURE(2.E-5),#18826,
'DISTANCE_ACCURACY_VALUE','Maximum Tolerance applied to model');
#18823=UNCERTAINTY_MEASURE_WITH_UNIT(LENGTH_MEASURE(2.23351470508855E-5),
#18826,'DISTANCE_ACCURACY_VALUE','Maximum Tolerance applied to model');
#18824=(
NAMED_UNIT(*)
SI_UNIT($,.STERADIAN.)
SOLID_ANGLE_UNIT()
);
#18825=(
NAMED_UNIT(*)
PLANE_ANGLE_UNIT()
SI_UNIT($,.RADIAN.)
);
#18826=(
LENGTH_UNIT()
NAMED_UNIT(*)
SI_UNIT($,.METRE.)
);
#18827=PRODUCT_DEFINITION_SHAPE('','',#18840);
#18828=PRODUCT_DEFINITION_SHAPE('','',#18841);
#18829=PRODUCT_DEFINITION_SHAPE(' ','NAUO PRDDFN',#125);
#18830=PRODUCT_DEFINITION_SHAPE('','',#18842);
#18831=PRODUCT_DEFINITION_SHAPE(' ','NAUO PRDDFN',#126);
#18832=PRODUCT_DEFINITION_SHAPE('','',#18843);
#18833=PRODUCT_DEFINITION_SHAPE(' ','NAUO PRDDFN',#127);
#18834=PRODUCT_DEFINITION_SHAPE('','',#18844);
#18835=PRODUCT_DEFINITION_SHAPE(' ','NAUO PRDDFN',#128);
#18836=PRODUCT_DEFINITION_SHAPE('','',#18845);
#18837=PRODUCT_DEFINITION_SHAPE(' ','NAUO PRDDFN',#129);
#18838=PRODUCT_DEFINITION_SHAPE('','',#18846);
#18839=PRODUCT_DEFINITION_SHAPE(' ','NAUO PRDDFN',#130);
#18840=PRODUCT_DEFINITION('','',#18854,#18847);
#18841=PRODUCT_DEFINITION('','',#18855,#18848);
#18842=PRODUCT_DEFINITION('','',#18856,#18849);
#18843=PRODUCT_DEFINITION('','',#18857,#18850);
#18844=PRODUCT_DEFINITION('','',#18858,#18851);
#18845=PRODUCT_DEFINITION('','',#18859,#18852);
#18846=PRODUCT_DEFINITION('','',#18860,#18853);
#18847=PRODUCT_DEFINITION_CONTEXT('',#18890,'design');
#18848=PRODUCT_DEFINITION_CONTEXT('',#18890,'design');
#18849=PRODUCT_DEFINITION_CONTEXT('',#18890,'design');
#18850=PRODUCT_DEFINITION_CONTEXT('',#18890,'design');
#18851=PRODUCT_DEFINITION_CONTEXT('',#18890,'design');
#18852=PRODUCT_DEFINITION_CONTEXT('',#18890,'design');
#18853=PRODUCT_DEFINITION_CONTEXT('',#18890,'design');
#18854=PRODUCT_DEFINITION_FORMATION_WITH_SPECIFIED_SOURCE('','',#18868,
 .NOT_KNOWN.);
#18855=PRODUCT_DEFINITION_FORMATION_WITH_SPECIFIED_SOURCE('','',#18869,
 .NOT_KNOWN.);
#18856=PRODUCT_DEFINITION_FORMATION_WITH_SPECIFIED_SOURCE('','',#18870,
 .NOT_KNOWN.);
#18857=PRODUCT_DEFINITION_FORMATION_WITH_SPECIFIED_SOURCE('','',#18871,
 .NOT_KNOWN.);
#18858=PRODUCT_DEFINITION_FORMATION_WITH_SPECIFIED_SOURCE('','',#18872,
 .NOT_KNOWN.);
#18859=PRODUCT_DEFINITION_FORMATION_WITH_SPECIFIED_SOURCE('','',#18873,
 .NOT_KNOWN.);
#18860=PRODUCT_DEFINITION_FORMATION_WITH_SPECIFIED_SOURCE('','',#18874,
 .NOT_KNOWN.);
#18861=PRODUCT_RELATED_PRODUCT_CATEGORY('','',(#18868));
#18862=PRODUCT_RELATED_PRODUCT_CATEGORY('','',(#18869));
#18863=PRODUCT_RELATED_PRODUCT_CATEGORY('','',(#18870));
#18864=PRODUCT_RELATED_PRODUCT_CATEGORY('','',(#18871));
#18865=PRODUCT_RELATED_PRODUCT_CATEGORY('','',(#18872));
#18866=PRODUCT_RELATED_PRODUCT_CATEGORY('','',(#18873));
#18867=PRODUCT_RELATED_PRODUCT_CATEGORY('','',(#18874));
#18868=PRODUCT('MAS-697','MAS-697','MAS-697',(#18882));
#18869=PRODUCT('cassette body__ DE    15749',
'cassette body__ DE    15749','cassette body__ DE    15749',(#18883));
#18870=PRODUCT('endcap2__ DE    22113','endcap2__ DE    22113',
'endcap2__ DE    22113',(#18884));
#18871=PRODUCT('endcap__ DE    14671','endcap__ DE    14671',
'endcap__ DE    14671',(#18885));
#18872=PRODUCT(
'angular contact ball bearing_68_bsi_BS 6267 ABB - 4815 - 18,SI,NC,18_
68__ DE    23193',
'angular contact ball bearing_68_bsi_BS 6267 ABB - 4815 - 18,SI,NC,18_
68__ DE    23193',
'angular contact ball bearing_68_bsi_BS 6267 ABB - 4815 - 18,SI,NC,18_
68__ DE    23193',(#18886));
#18873=PRODUCT(
'angular contact ball bearing_68_bsi_BS 6267 ABB - 4815 - 18,SI,NC,18_
68__ DE    23193',
'angular contact ball bearing_68_bsi_BS 6267 ABB - 4815 - 18,SI,NC,18_
68__ DE    23193',
'angular contact ball bearing_68_bsi_BS 6267 ABB - 4815 - 18,SI,NC,18_
68__ DE    23193',(#18887));
#18874=PRODUCT('HubBody__ DE       35','HubBody__ DE       35',
'HubBody__ DE       35',(#18888));
#18875=PRODUCT_CATEGORY('','');
#18876=PRODUCT_CATEGORY('','');
#18877=PRODUCT_CATEGORY('','');
#18878=PRODUCT_CATEGORY('','');
#18879=PRODUCT_CATEGORY('','');
#18880=PRODUCT_CATEGORY('','');
#18881=PRODUCT_CATEGORY('','');
#18882=PRODUCT_CONTEXT('',#18890,'mechanical');
#18883=PRODUCT_CONTEXT('',#18890,'mechanical');
#18884=PRODUCT_CONTEXT('',#18890,'mechanical');
#18885=PRODUCT_CONTEXT('',#18890,'mechanical');
#18886=PRODUCT_CONTEXT('',#18890,'mechanical');
#18887=PRODUCT_CONTEXT('',#18890,'mechanical');
#18888=PRODUCT_CONTEXT('',#18890,'mechanical');
#18889=APPLICATION_PROTOCOL_DEFINITION('international standard',
'ap242_managed_model_based_3d_engineering',2020,#18890);
#18890=APPLICATION_CONTEXT('managed model based 3d engineering');
ENDSEC;
END-ISO-10303-21;
